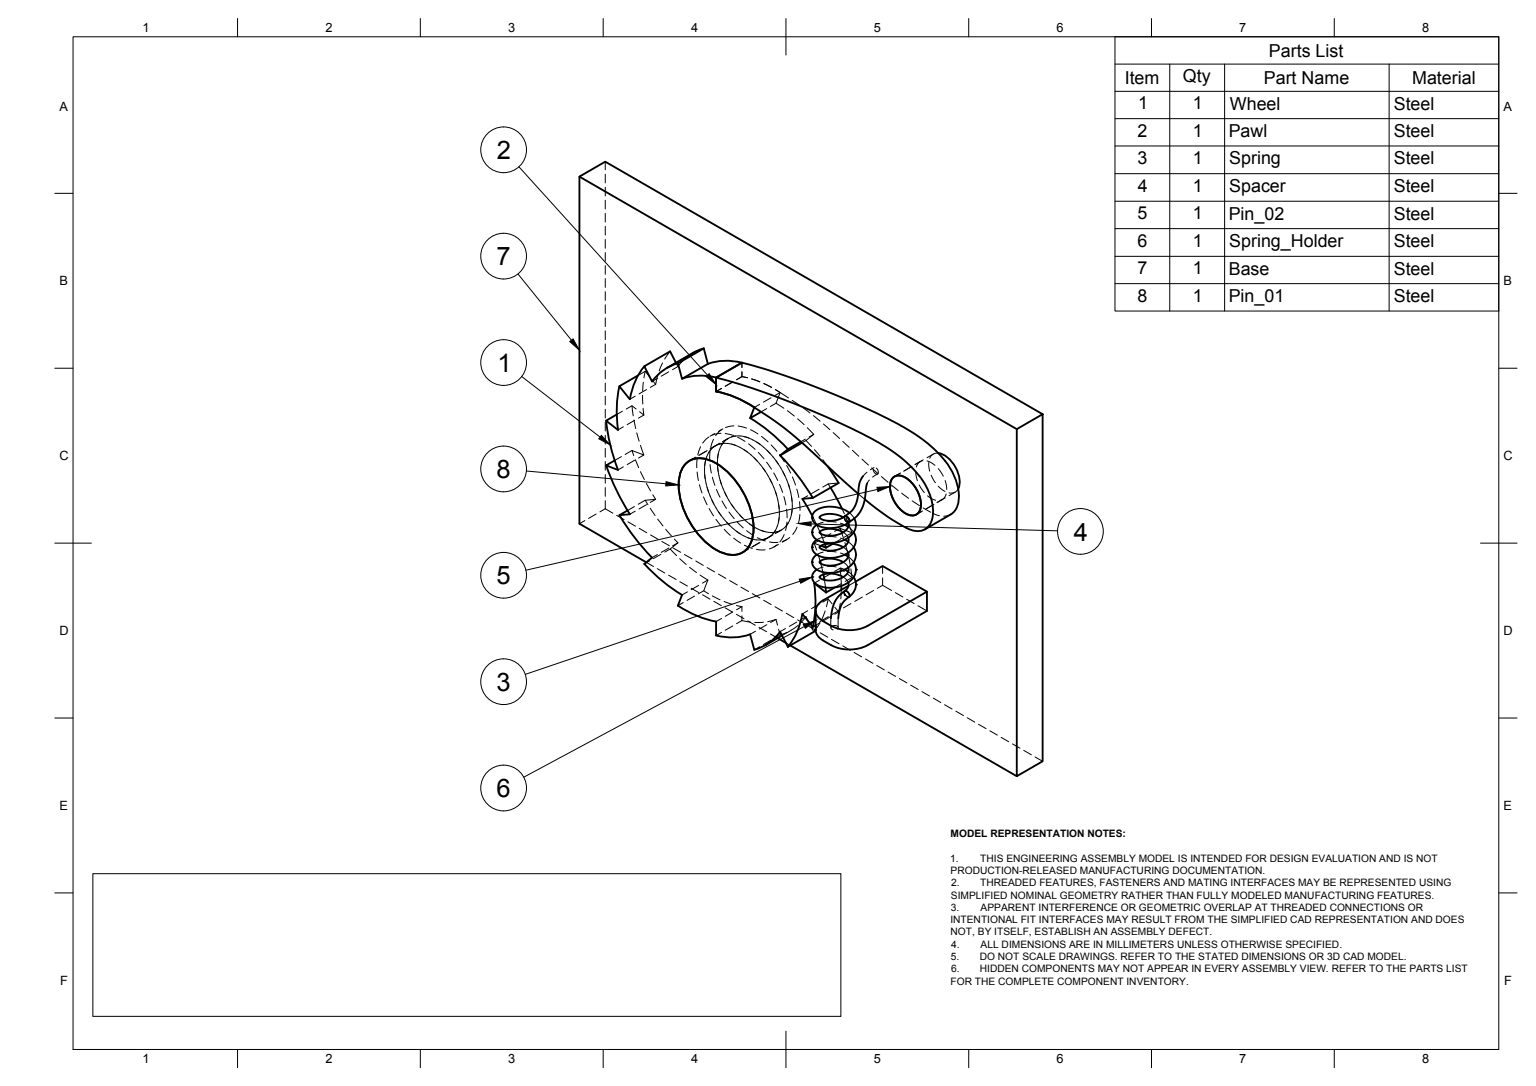
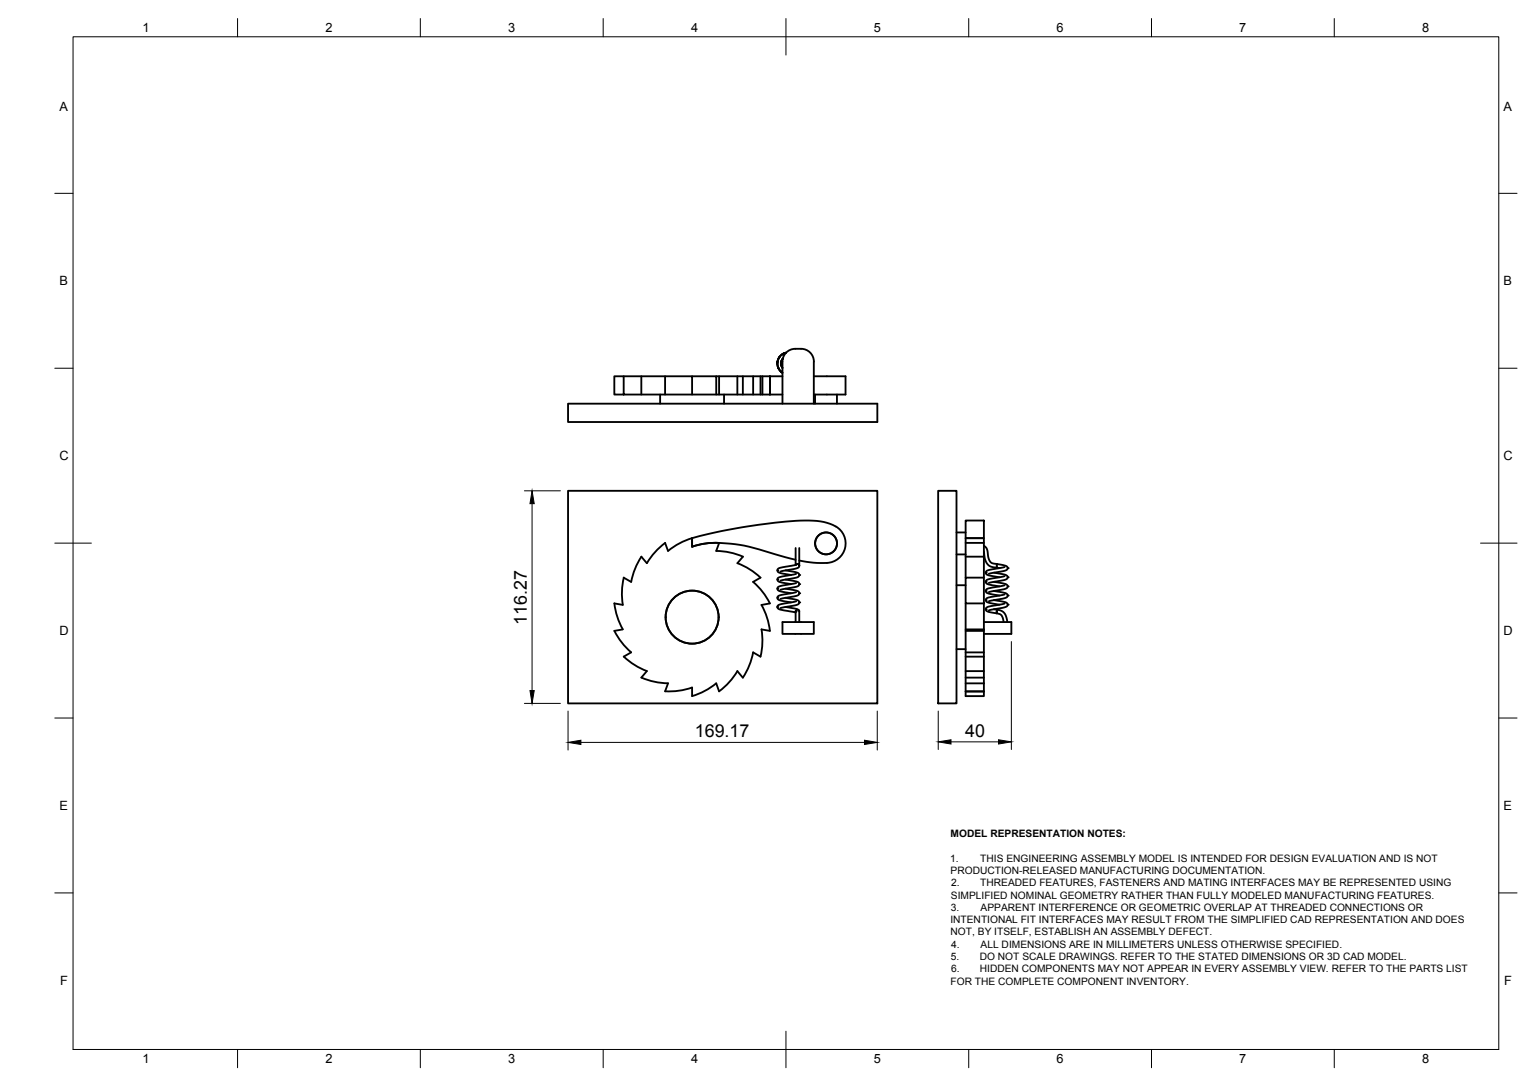
ISO-10303-21;
HEADER;
/* Generated by software containing ST-Developer
 * from STEP Tools, Inc. (www.steptools.com) 
 */

FILE_DESCRIPTION(
/* description */ (''),
/* implementation_level */ '2;1');

FILE_NAME(
/* name */ 'BR-055',
/* time_stamp */ '2026-09-20T22:38:01+06:00',
/* author */ (''),
/* organization */ (''),
/* preprocessor_version */ 'ST-DEVELOPER v20.2',
/* originating_system */ 'Autodesk Translation Framework v15.15.0.0',
/* authorisation */ '');

FILE_SCHEMA (('AUTOMOTIVE_DESIGN { 1 0 10303 214 3 1 1 }'));
ENDSEC;

DATA;
#10=MECHANICAL_DESIGN_GEOMETRIC_PRESENTATION_REPRESENTATION('',(#84,#85,
#86,#87,#88,#89,#90,#91),#4079);
#11=ITEM_DEFINED_TRANSFORMATION($,$,#1541,#1690);
#12=ITEM_DEFINED_TRANSFORMATION($,$,#1619,#1691);
#13=ITEM_DEFINED_TRANSFORMATION($,$,#1632,#1692);
#14=ITEM_DEFINED_TRANSFORMATION($,$,#1649,#1693);
#15=ITEM_DEFINED_TRANSFORMATION($,$,#1658,#1694);
#16=ITEM_DEFINED_TRANSFORMATION($,$,#1664,#1695);
#17=ITEM_DEFINED_TRANSFORMATION($,$,#1677,#1696);
#18=ITEM_DEFINED_TRANSFORMATION($,$,#1684,#1697);
#19=(
REPRESENTATION_RELATIONSHIP($,$,#4111,#4110)
REPRESENTATION_RELATIONSHIP_WITH_TRANSFORMATION(#11)
SHAPE_REPRESENTATION_RELATIONSHIP()
);
#20=(
REPRESENTATION_RELATIONSHIP($,$,#4112,#4110)
REPRESENTATION_RELATIONSHIP_WITH_TRANSFORMATION(#12)
SHAPE_REPRESENTATION_RELATIONSHIP()
);
#21=(
REPRESENTATION_RELATIONSHIP($,$,#4113,#4110)
REPRESENTATION_RELATIONSHIP_WITH_TRANSFORMATION(#13)
SHAPE_REPRESENTATION_RELATIONSHIP()
);
#22=(
REPRESENTATION_RELATIONSHIP($,$,#4114,#4110)
REPRESENTATION_RELATIONSHIP_WITH_TRANSFORMATION(#14)
SHAPE_REPRESENTATION_RELATIONSHIP()
);
#23=(
REPRESENTATION_RELATIONSHIP($,$,#4115,#4110)
REPRESENTATION_RELATIONSHIP_WITH_TRANSFORMATION(#15)
SHAPE_REPRESENTATION_RELATIONSHIP()
);
#24=(
REPRESENTATION_RELATIONSHIP($,$,#4116,#4110)
REPRESENTATION_RELATIONSHIP_WITH_TRANSFORMATION(#16)
SHAPE_REPRESENTATION_RELATIONSHIP()
);
#25=(
REPRESENTATION_RELATIONSHIP($,$,#4117,#4110)
REPRESENTATION_RELATIONSHIP_WITH_TRANSFORMATION(#17)
SHAPE_REPRESENTATION_RELATIONSHIP()
);
#26=(
REPRESENTATION_RELATIONSHIP($,$,#4118,#4110)
REPRESENTATION_RELATIONSHIP_WITH_TRANSFORMATION(#18)
SHAPE_REPRESENTATION_RELATIONSHIP()
);
#27=CONTEXT_DEPENDENT_SHAPE_REPRESENTATION(#19,#4102);
#28=CONTEXT_DEPENDENT_SHAPE_REPRESENTATION(#20,#4103);
#29=CONTEXT_DEPENDENT_SHAPE_REPRESENTATION(#21,#4104);
#30=CONTEXT_DEPENDENT_SHAPE_REPRESENTATION(#22,#4105);
#31=CONTEXT_DEPENDENT_SHAPE_REPRESENTATION(#23,#4106);
#32=CONTEXT_DEPENDENT_SHAPE_REPRESENTATION(#24,#4107);
#33=CONTEXT_DEPENDENT_SHAPE_REPRESENTATION(#25,#4108);
#34=CONTEXT_DEPENDENT_SHAPE_REPRESENTATION(#26,#4109);
#35=NEXT_ASSEMBLY_USAGE_OCCURRENCE('Wheel:1','Wheel:1','Wheel:1',#4120,
#4121,'Wheel:1');
#36=NEXT_ASSEMBLY_USAGE_OCCURRENCE('Pawl:1','Pawl:1','Pawl:1',#4120,#4122,
'Pawl:1');
#37=NEXT_ASSEMBLY_USAGE_OCCURRENCE('Spring:1','Spring:1','Spring:1',#4120,
#4123,'Spring:1');
#38=NEXT_ASSEMBLY_USAGE_OCCURRENCE('Spacer:1','Spacer:1','Spacer:1',#4120,
#4124,'Spacer:1');
#39=NEXT_ASSEMBLY_USAGE_OCCURRENCE('Pin_02:1','Pin_02:1','Pin_02:1',#4120,
#4125,'Pin_02:1');
#40=NEXT_ASSEMBLY_USAGE_OCCURRENCE('Spring_Holder:1','Spring_Holder:1',
'Spring_Holder:1',#4120,#4126,'Spring_Holder:1');
#41=NEXT_ASSEMBLY_USAGE_OCCURRENCE('Base:1','Base:1','Base:1',#4120,#4127,
'Base:1');
#42=NEXT_ASSEMBLY_USAGE_OCCURRENCE('Pin_01:1','Pin_01:1','Pin_01:1',#4120,
#4128,'Pin_01:1');
#43=B_SPLINE_CURVE_WITH_KNOTS('',3,(#2659,#2660,#2661,#2662,#2663,#2664,
#2665,#2666,#2667,#2668,#2669,#2670,#2671,#2672,#2673,#2674,#2675,#2676,
#2677,#2678,#2679,#2680,#2681,#2682,#2683,#2684,#2685,#2686),
 .UNSPECIFIED.,.F.,.F.,(4,3,3,3,3,3,3,3,3,4),(-0.465553767595507,-0.45230342916427,
-0.438736142747031,-0.431079433868877,-0.417558478811202,-0.404199900672923,
-0.391686604552913,-0.378322214394046,-0.374830772248012,-0.369773118077988),
 .UNSPECIFIED.);
#44=B_SPLINE_CURVE_WITH_KNOTS('',3,(#2688,#2689,#2690,#2691,#2692,#2693,
#2694,#2695,#2696,#2697),.UNSPECIFIED.,.F.,.F.,(4,2,2,2,4),(-0.09742200167385,
-0.0775242929113368,-0.0386624365460309,0.,0.00241811618144354),
 .UNSPECIFIED.);
#45=B_SPLINE_CURVE_WITH_KNOTS('',3,(#2702,#2703,#2704,#2705,#2706,#2707,
#2708,#2709,#2710,#2711),.UNSPECIFIED.,.F.,.F.,(4,3,3,4),(-0.657219142658169,
-0.648664678619421,-0.598426048115365,-0.569492481999336),.UNSPECIFIED.);
#46=B_SPLINE_CURVE_WITH_KNOTS('',3,(#2712,#2713,#2714,#2715,#2716,#2717,
#2718,#2719,#2720,#2721),.UNSPECIFIED.,.F.,.F.,(4,3,3,4),(-0.489269526390867,
-0.47602824474659,-0.470821216724862,-0.465553767595507),.UNSPECIFIED.);
#47=B_SPLINE_CURVE_WITH_KNOTS('',3,(#2723,#2724,#2725,#2726,#2727,#2728,
#2729,#2730,#2731),.UNSPECIFIED.,.F.,.F.,(4,1,1,1,1,1,4),(0.0132171477861262,
0.142857142857143,0.285714285714286,0.428571428571429,0.571428571428571,
0.857142857142857,1.),.UNSPECIFIED.);
#48=B_SPLINE_CURVE_WITH_KNOTS('',3,(#3403,#3404,#3405,#3406,#3407,#3408,
#3409,#3410,#3411,#3412,#3413,#3414,#3415,#3416,#3417,#3418,#3419,#3420,
#3421,#3422,#3423,#3424,#3425),.UNSPECIFIED.,.F.,.F.,(4,2,3,2,2,2,2,2,2,
2,4),(0.587267836178956,0.604560146171109,0.626248329271999,0.664698946888708,
0.70347541138122,0.74264809527987,0.78210152700143,0.821492769940296,0.860375715352057,
0.898588405045022,0.900352617840992),.UNSPECIFIED.);
#49=B_SPLINE_CURVE_WITH_KNOTS('',3,(#3427,#3428,#3429,#3430,#3431,#3432,
#3433,#3434,#3435,#3436,#3437,#3438,#3439,#3440,#3441,#3442,#3443,#3444,
#3445,#3446,#3447,#3448,#3449,#3450,#3451,#3452,#3453,#3454,#3455,#3456,
#3457,#3458,#3459,#3460,#3461,#3462,#3463,#3464,#3465,#3466,#3467,#3468,
#3469,#3470,#3471,#3472,#3473,#3474,#3475,#3476,#3477,#3478,#3479,#3480,
#3481,#3482,#3483,#3484,#3485,#3486,#3487,#3488,#3489,#3490,#3491,#3492,
#3493),.UNSPECIFIED.,.F.,.F.,(4,1,1,1,1,1,1,1,1,1,1,1,1,1,1,1,1,1,1,1,1,
1,1,1,1,1,1,1,1,1,1,1,1,1,1,1,1,1,1,1,1,1,1,1,1,1,1,1,1,1,1,1,1,1,1,1,1,
1,1,1,1,1,1,1,4),(0.,0.464577110944849,0.95586837165839,1.44715963237193,
1.93845089308547,2.42974215379901,2.92103341451255,3.41232467522609,3.90361593593964,
4.39490719665318,4.88619845736672,5.37748971808026,5.8687809787938,6.36007223950734,
6.85136350022088,7.34265476093442,7.83394602164796,8.3252372823615,8.81652854307505,
9.30781980378859,9.79911106450213,10.2904023252157,10.7816935859292,11.2729848466427,
11.7642761073563,12.2555673680698,12.7468586287834,13.2381498894969,13.7294411502105,
14.220732410924,14.7120236716375,15.2033149323511,15.6946061930646,16.1858974537782,
16.6771887144917,17.1684799752052,17.6597712359188,18.1510624966323,18.6423537573459,
19.1336450180594,19.6249362787729,20.1162275394865,20.6075188002,21.0988100609136,
21.5901013216271,22.0813925823407,22.5726838430542,23.0639751037677,23.5552663644813,
24.0465576251948,24.5378488859084,25.0291401466219,25.5204314073354,26.011722668049,
26.5030139287625,26.9943051894761,27.4855964501896,27.9768877109031,28.4681789716167,
28.9594702323302,29.4507614930438,29.9420527537573,30.4333440144708,30.9246352751844,
31.4159265358979),.UNSPECIFIED.);
#50=B_SPLINE_CURVE_WITH_KNOTS('',3,(#3495,#3496,#3497,#3498,#3499,#3500,
#3501,#3502,#3503,#3504,#3505,#3506,#3507,#3508,#3509,#3510,#3511,#3512,
#3513,#3514),.UNSPECIFIED.,.F.,.F.,(4,2,2,2,2,2,2,2,2,4),(-0.313052705156199,
-0.292609441796844,-0.272153993775093,-0.233472325120928,-0.194370984993977,
-0.154905297587714,-0.115391052867927,-0.0763129985395409,-0.0379453287021336,
0.),.UNSPECIFIED.);
#51=B_SPLINE_CURVE_WITH_KNOTS('',3,(#3516,#3517,#3518,#3519,#3520,#3521,
#3522,#3523,#3524,#3525,#3526,#3527,#3528,#3529,#3530,#3531),
 .UNSPECIFIED.,.F.,.F.,(4,3,3,3,3,4),(-0.0024248849541149,0.,0.0138283319525736,
0.0273768962823761,0.0362935842092716,0.0434201122759664),.UNSPECIFIED.);
#52=B_SPLINE_CURVE_WITH_KNOTS('',3,(#3533,#3534,#3535,#3536,#3537,#3538),
 .UNSPECIFIED.,.F.,.F.,(4,2,4),(-0.0515505060017679,-0.0391387739403107,
0.),.UNSPECIFIED.);
#53=B_SPLINE_CURVE_WITH_KNOTS('',3,(#3542,#3543,#3544,#3545,#3546,#3547,
#3548,#3549,#3550,#3551,#3552,#3553,#3554,#3555,#3556,#3557,#3558,#3559,
#3560,#3561),.UNSPECIFIED.,.F.,.F.,(4,2,2,2,2,2,2,2,2,4),(-0.313052705156207,
-0.29260944179685,-0.272153993775096,-0.233472325120924,-0.194370984993967,
-0.154905297587702,-0.11539105286792,-0.0763129985395404,-0.0379453287021338,
0.),.UNSPECIFIED.);
#54=B_SPLINE_CURVE_WITH_KNOTS('',3,(#3563,#3564,#3565,#3566,#3567,#3568,
#3569,#3570,#3571,#3572,#3573,#3574,#3575,#3576,#3577,#3578,#3579,#3580,
#3581,#3582,#3583,#3584,#3585,#3586,#3587,#3588,#3589,#3590,#3591,#3592,
#3593,#3594,#3595,#3596),.UNSPECIFIED.,.F.,.F.,(4,3,3,3,3,3,3,3,3,3,3,4),
(0.377352254196932,0.390588465654341,0.403867575958707,0.41718187397498,
0.429352359462404,0.437218808334642,0.450427222970435,0.463782588613302,
0.468146972739535,0.481501401691605,0.494833441685106,0.497267224677679),
 .UNSPECIFIED.);
#55=B_SPLINE_CURVE_WITH_KNOTS('',3,(#3600,#3601,#3602,#3603,#3604,#3605,
#3606,#3607,#3608,#3609,#3610,#3611,#3612,#3613,#3614,#3615,#3616,#3617,
#3618,#3619,#3620,#3621,#3622,#3623,#3624,#3625,#3626,#3627),
 .UNSPECIFIED.,.F.,.F.,(4,3,3,3,3,3,3,3,3,4),(0.458621120799817,0.464048968999107,
0.469643578756217,0.482746851650584,0.496256676637028,0.508878670584022,
0.522421915099756,0.535791652499991,0.548459753273671,0.554671659389392),
 .UNSPECIFIED.);
#56=B_SPLINE_CURVE_WITH_KNOTS('',3,(#3888,#3889,#3890,#3891,#3892,#3893,
#3894,#3895,#3896,#3897),.UNSPECIFIED.,.F.,.F.,(4,3,3,4),(-0.319964114535563,
-0.319531325306217,-0.229500308639694,-0.144878157103041),.UNSPECIFIED.);
#57=B_SPLINE_CURVE_WITH_KNOTS('',3,(#3900,#3901,#3902,#3903,#3904,#3905,
#3906,#3907,#3908,#3909,#3910,#3911,#3912,#3913,#3914,#3915,#3916,#3917,
#3918,#3919,#3920,#3921,#3922,#3923),.UNSPECIFIED.,.F.,.F.,(4,1,1,1,1,1,
1,1,1,1,1,1,1,1,1,1,1,1,1,1,1,4),(0.,0.025,0.05,0.1,0.15,0.175,0.2,0.3,
0.4,0.425,0.45,0.5,0.55,0.575,0.6,0.7,0.75,0.8,0.825,0.85,0.9,1.),
 .UNSPECIFIED.);
#58=B_SPLINE_SURFACE_WITH_KNOTS('',3,3,((#2567,#2568,#2569,#2570,#2571,
#2572,#2573,#2574,#2575),(#2576,#2577,#2578,#2579,#2580,#2581,#2582,#2583,
#2584),(#2585,#2586,#2587,#2588,#2589,#2590,#2591,#2592,#2593),(#2594,#2595,
#2596,#2597,#2598,#2599,#2600,#2601,#2602),(#2603,#2604,#2605,#2606,#2607,
#2608,#2609,#2610,#2611),(#2612,#2613,#2614,#2615,#2616,#2617,#2618,#2619,
#2620),(#2621,#2622,#2623,#2624,#2625,#2626,#2627,#2628,#2629),(#2630,#2631,
#2632,#2633,#2634,#2635,#2636,#2637,#2638),(#2639,#2640,#2641,#2642,#2643,
#2644,#2645,#2646,#2647),(#2648,#2649,#2650,#2651,#2652,#2653,#2654,#2655,
#2656)),.UNSPECIFIED.,.T.,.F.,.F.,(4,1,1,1,1,1,1,4),(4,1,1,1,1,1,4),(-3.14159265359034,
-2.2439947525646,-1.34639685153886,-0.448798950513122,0.448798950512615,
1.34639685153835,2.24399475256409,3.14159265358983),(0.,0.142857142857143,
0.285714285714286,0.428571428571429,0.571428571428571,0.857142857142857,
1.),.UNSPECIFIED.);
#59=B_SPLINE_SURFACE_WITH_KNOTS('',3,3,((#2733,#2734,#2735,#2736,#2737,
#2738,#2739,#2740,#2741,#2742,#2743,#2744,#2745,#2746,#2747,#2748,#2749,
#2750,#2751,#2752,#2753,#2754,#2755,#2756,#2757,#2758,#2759,#2760,#2761,
#2762,#2763,#2764,#2765,#2766,#2767,#2768,#2769,#2770,#2771,#2772,#2773,
#2774,#2775,#2776,#2777,#2778,#2779,#2780,#2781,#2782,#2783,#2784,#2785,
#2786,#2787,#2788,#2789,#2790,#2791,#2792,#2793,#2794,#2795,#2796,#2797,
#2798,#2799),(#2800,#2801,#2802,#2803,#2804,#2805,#2806,#2807,#2808,#2809,
#2810,#2811,#2812,#2813,#2814,#2815,#2816,#2817,#2818,#2819,#2820,#2821,
#2822,#2823,#2824,#2825,#2826,#2827,#2828,#2829,#2830,#2831,#2832,#2833,
#2834,#2835,#2836,#2837,#2838,#2839,#2840,#2841,#2842,#2843,#2844,#2845,
#2846,#2847,#2848,#2849,#2850,#2851,#2852,#2853,#2854,#2855,#2856,#2857,
#2858,#2859,#2860,#2861,#2862,#2863,#2864,#2865,#2866),(#2867,#2868,#2869,
#2870,#2871,#2872,#2873,#2874,#2875,#2876,#2877,#2878,#2879,#2880,#2881,
#2882,#2883,#2884,#2885,#2886,#2887,#2888,#2889,#2890,#2891,#2892,#2893,
#2894,#2895,#2896,#2897,#2898,#2899,#2900,#2901,#2902,#2903,#2904,#2905,
#2906,#2907,#2908,#2909,#2910,#2911,#2912,#2913,#2914,#2915,#2916,#2917,
#2918,#2919,#2920,#2921,#2922,#2923,#2924,#2925,#2926,#2927,#2928,#2929,
#2930,#2931,#2932,#2933),(#2934,#2935,#2936,#2937,#2938,#2939,#2940,#2941,
#2942,#2943,#2944,#2945,#2946,#2947,#2948,#2949,#2950,#2951,#2952,#2953,
#2954,#2955,#2956,#2957,#2958,#2959,#2960,#2961,#2962,#2963,#2964,#2965,
#2966,#2967,#2968,#2969,#2970,#2971,#2972,#2973,#2974,#2975,#2976,#2977,
#2978,#2979,#2980,#2981,#2982,#2983,#2984,#2985,#2986,#2987,#2988,#2989,
#2990,#2991,#2992,#2993,#2994,#2995,#2996,#2997,#2998,#2999,#3000),(#3001,
#3002,#3003,#3004,#3005,#3006,#3007,#3008,#3009,#3010,#3011,#3012,#3013,
#3014,#3015,#3016,#3017,#3018,#3019,#3020,#3021,#3022,#3023,#3024,#3025,
#3026,#3027,#3028,#3029,#3030,#3031,#3032,#3033,#3034,#3035,#3036,#3037,
#3038,#3039,#3040,#3041,#3042,#3043,#3044,#3045,#3046,#3047,#3048,#3049,
#3050,#3051,#3052,#3053,#3054,#3055,#3056,#3057,#3058,#3059,#3060,#3061,
#3062,#3063,#3064,#3065,#3066,#3067),(#3068,#3069,#3070,#3071,#3072,#3073,
#3074,#3075,#3076,#3077,#3078,#3079,#3080,#3081,#3082,#3083,#3084,#3085,
#3086,#3087,#3088,#3089,#3090,#3091,#3092,#3093,#3094,#3095,#3096,#3097,
#3098,#3099,#3100,#3101,#3102,#3103,#3104,#3105,#3106,#3107,#3108,#3109,
#3110,#3111,#3112,#3113,#3114,#3115,#3116,#3117,#3118,#3119,#3120,#3121,
#3122,#3123,#3124,#3125,#3126,#3127,#3128,#3129,#3130,#3131,#3132,#3133,
#3134),(#3135,#3136,#3137,#3138,#3139,#3140,#3141,#3142,#3143,#3144,#3145,
#3146,#3147,#3148,#3149,#3150,#3151,#3152,#3153,#3154,#3155,#3156,#3157,
#3158,#3159,#3160,#3161,#3162,#3163,#3164,#3165,#3166,#3167,#3168,#3169,
#3170,#3171,#3172,#3173,#3174,#3175,#3176,#3177,#3178,#3179,#3180,#3181,
#3182,#3183,#3184,#3185,#3186,#3187,#3188,#3189,#3190,#3191,#3192,#3193,
#3194,#3195,#3196,#3197,#3198,#3199,#3200,#3201),(#3202,#3203,#3204,#3205,
#3206,#3207,#3208,#3209,#3210,#3211,#3212,#3213,#3214,#3215,#3216,#3217,
#3218,#3219,#3220,#3221,#3222,#3223,#3224,#3225,#3226,#3227,#3228,#3229,
#3230,#3231,#3232,#3233,#3234,#3235,#3236,#3237,#3238,#3239,#3240,#3241,
#3242,#3243,#3244,#3245,#3246,#3247,#3248,#3249,#3250,#3251,#3252,#3253,
#3254,#3255,#3256,#3257,#3258,#3259,#3260,#3261,#3262,#3263,#3264,#3265,
#3266,#3267,#3268),(#3269,#3270,#3271,#3272,#3273,#3274,#3275,#3276,#3277,
#3278,#3279,#3280,#3281,#3282,#3283,#3284,#3285,#3286,#3287,#3288,#3289,
#3290,#3291,#3292,#3293,#3294,#3295,#3296,#3297,#3298,#3299,#3300,#3301,
#3302,#3303,#3304,#3305,#3306,#3307,#3308,#3309,#3310,#3311,#3312,#3313,
#3314,#3315,#3316,#3317,#3318,#3319,#3320,#3321,#3322,#3323,#3324,#3325,
#3326,#3327,#3328,#3329,#3330,#3331,#3332,#3333,#3334,#3335),(#3336,#3337,
#3338,#3339,#3340,#3341,#3342,#3343,#3344,#3345,#3346,#3347,#3348,#3349,
#3350,#3351,#3352,#3353,#3354,#3355,#3356,#3357,#3358,#3359,#3360,#3361,
#3362,#3363,#3364,#3365,#3366,#3367,#3368,#3369,#3370,#3371,#3372,#3373,
#3374,#3375,#3376,#3377,#3378,#3379,#3380,#3381,#3382,#3383,#3384,#3385,
#3386,#3387,#3388,#3389,#3390,#3391,#3392,#3393,#3394,#3395,#3396,#3397,
#3398,#3399,#3400,#3401,#3402)),.UNSPECIFIED.,.T.,.F.,.F.,(4,1,1,1,1,1,
1,4),(4,1,1,1,1,1,1,1,1,1,1,1,1,1,1,1,1,1,1,1,1,1,1,1,1,1,1,1,1,1,1,1,1,
1,1,1,1,1,1,1,1,1,1,1,1,1,1,1,1,1,1,1,1,1,1,1,1,1,1,1,1,1,1,1,4),(-3.14159265358979,
-2.24399475256414,-1.34639685153848,-0.448798950512828,0.448798950512828,
1.34639685153848,2.24399475256414,3.14159265358979),(-0.0267141497686917,
0.464577110944849,0.95586837165839,1.44715963237193,1.93845089308547,2.42974215379901,
2.92103341451255,3.41232467522609,3.90361593593964,4.39490719665318,4.88619845736672,
5.37748971808026,5.8687809787938,6.36007223950734,6.85136350022088,7.34265476093442,
7.83394602164796,8.3252372823615,8.81652854307505,9.30781980378859,9.79911106450213,
10.2904023252157,10.7816935859292,11.2729848466427,11.7642761073563,12.2555673680698,
12.7468586287834,13.2381498894969,13.7294411502105,14.220732410924,14.7120236716375,
15.2033149323511,15.6946061930646,16.1858974537782,16.6771887144917,17.1684799752052,
17.6597712359188,18.1510624966323,18.6423537573459,19.1336450180594,19.6249362787729,
20.1162275394865,20.6075188002,21.0988100609136,21.5901013216271,22.0813925823407,
22.5726838430542,23.0639751037677,23.5552663644813,24.0465576251948,24.5378488859084,
25.0291401466219,25.5204314073354,26.011722668049,26.5030139287625,26.9943051894761,
27.4855964501896,27.9768877109031,28.4681789716167,28.9594702323302,29.4507614930438,
29.9420527537573,30.4333440144708,30.9246352751844,31.4159265358979),
 .UNSPECIFIED.);
#60=B_SPLINE_SURFACE_WITH_KNOTS('',3,3,((#3628,#3629,#3630,#3631,#3632,
#3633,#3634,#3635,#3636,#3637,#3638,#3639,#3640,#3641,#3642,#3643,#3644,
#3645,#3646,#3647,#3648,#3649,#3650,#3651,#3652,#3653),(#3654,#3655,#3656,
#3657,#3658,#3659,#3660,#3661,#3662,#3663,#3664,#3665,#3666,#3667,#3668,
#3669,#3670,#3671,#3672,#3673,#3674,#3675,#3676,#3677,#3678,#3679),(#3680,
#3681,#3682,#3683,#3684,#3685,#3686,#3687,#3688,#3689,#3690,#3691,#3692,
#3693,#3694,#3695,#3696,#3697,#3698,#3699,#3700,#3701,#3702,#3703,#3704,
#3705),(#3706,#3707,#3708,#3709,#3710,#3711,#3712,#3713,#3714,#3715,#3716,
#3717,#3718,#3719,#3720,#3721,#3722,#3723,#3724,#3725,#3726,#3727,#3728,
#3729,#3730,#3731),(#3732,#3733,#3734,#3735,#3736,#3737,#3738,#3739,#3740,
#3741,#3742,#3743,#3744,#3745,#3746,#3747,#3748,#3749,#3750,#3751,#3752,
#3753,#3754,#3755,#3756,#3757),(#3758,#3759,#3760,#3761,#3762,#3763,#3764,
#3765,#3766,#3767,#3768,#3769,#3770,#3771,#3772,#3773,#3774,#3775,#3776,
#3777,#3778,#3779,#3780,#3781,#3782,#3783),(#3784,#3785,#3786,#3787,#3788,
#3789,#3790,#3791,#3792,#3793,#3794,#3795,#3796,#3797,#3798,#3799,#3800,
#3801,#3802,#3803,#3804,#3805,#3806,#3807,#3808,#3809),(#3810,#3811,#3812,
#3813,#3814,#3815,#3816,#3817,#3818,#3819,#3820,#3821,#3822,#3823,#3824,
#3825,#3826,#3827,#3828,#3829,#3830,#3831,#3832,#3833,#3834,#3835),(#3836,
#3837,#3838,#3839,#3840,#3841,#3842,#3843,#3844,#3845,#3846,#3847,#3848,
#3849,#3850,#3851,#3852,#3853,#3854,#3855,#3856,#3857,#3858,#3859,#3860,
#3861),(#3862,#3863,#3864,#3865,#3866,#3867,#3868,#3869,#3870,#3871,#3872,
#3873,#3874,#3875,#3876,#3877,#3878,#3879,#3880,#3881,#3882,#3883,#3884,
#3885,#3886,#3887)),.UNSPECIFIED.,.T.,.F.,.F.,(4,1,1,1,1,1,1,4),(4,2,1,
1,1,1,1,1,1,1,1,1,1,1,1,1,1,1,1,1,1,1,4),(-3.14159265358979,-2.24399475256414,
-1.34639685153848,-0.448798950512828,0.448798950512828,1.34639685153848,
2.24399475256414,3.14159265358979),(-0.00680747846147418,0.,0.025,0.05,
0.1,0.15,0.175,0.2,0.3,0.4,0.425,0.45,0.5,0.55,0.575,0.6,0.7,0.75,0.8,0.825,
0.85,0.9,1.),.UNSPECIFIED.);
#61=B_SPLINE_SURFACE_WITH_KNOTS('',3,3,((#3925,#3926,#3927,#3928),(#3929,
#3930,#3931,#3932),(#3933,#3934,#3935,#3936),(#3937,#3938,#3939,#3940),
(#3941,#3942,#3943,#3944)),.UNSPECIFIED.,.F.,.F.,.F.,(4,1,4),(4,4),(-0.950877784735382,
-0.352362581588169,0.246152621559044),(-0.0375396701634702,0.),
 .UNSPECIFIED.);
#62=(
BOUNDED_CURVE()
B_SPLINE_CURVE(5,(#2402,#2403,#2404,#2405,#2406,#2407,#2408,#2409,#2410,
#2411,#2412,#2413,#2414,#2415,#2416,#2417,#2418,#2419,#2420,#2421),
 .UNSPECIFIED.,.F.,.F.)
B_SPLINE_CURVE_WITH_KNOTS((6,1,1,1,1,1,1,1,1,1,1,1,1,1,1,6),(0.,0.0666666666666667,
0.133333333333333,0.2,0.266666666666667,0.333333333333333,0.4,0.466666666666667,
0.533333333333333,0.6,0.666666666666667,0.733333333333333,0.8,0.866666666666667,
0.933333333333333,1.),.UNSPECIFIED.)
CURVE()
GEOMETRIC_REPRESENTATION_ITEM()
RATIONAL_B_SPLINE_CURVE((1.,1.,1.,1.,1.,1.,1.,1.,1.,1.,1.,1.,1.,1.,1.,1.,
1.,1.,1.,1.))
REPRESENTATION_ITEM('')
);
#63=(
BOUNDED_CURVE()
B_SPLINE_CURVE(5,(#2425,#2426,#2427,#2428,#2429,#2430,#2431,#2432,#2433,
#2434,#2435,#2436,#2437,#2438,#2439,#2440,#2441,#2442,#2443,#2444),
 .UNSPECIFIED.,.F.,.F.)
B_SPLINE_CURVE_WITH_KNOTS((6,1,1,1,1,1,1,1,1,1,1,1,1,1,1,6),(-1.,-0.933333333333333,
-0.866666666666667,-0.8,-0.733333333333333,-0.666666666666667,-0.6,-0.533333333333333,
-0.466666666666667,-0.4,-0.333333333333333,-0.266666666666667,-0.2,-0.133333333333333,
-0.0666666666666667,0.),.UNSPECIFIED.)
CURVE()
GEOMETRIC_REPRESENTATION_ITEM()
RATIONAL_B_SPLINE_CURVE((1.,1.,1.,1.,1.,1.,1.,1.,1.,1.,1.,1.,1.,1.,1.,1.,
1.,1.,1.,1.))
REPRESENTATION_ITEM('')
);
#64=(
BOUNDED_CURVE()
B_SPLINE_CURVE(5,(#2503,#2504,#2505,#2506,#2507,#2508,#2509,#2510,#2511,
#2512,#2513,#2514,#2515,#2516,#2517,#2518,#2519,#2520,#2521,#2522,#2523,
#2524,#2525,#2526,#2527),.UNSPECIFIED.,.F.,.F.)
B_SPLINE_CURVE_WITH_KNOTS((6,1,1,1,1,1,1,1,1,1,1,1,1,1,1,1,1,1,1,1,6),(0.,
0.05,0.1,0.15,0.2,0.25,0.3,0.35,0.4,0.45,0.5,0.55,0.6,0.65,0.7,0.75,0.8,
0.85,0.9,0.95,1.),.UNSPECIFIED.)
CURVE()
GEOMETRIC_REPRESENTATION_ITEM()
RATIONAL_B_SPLINE_CURVE((1.,1.,1.,1.,1.,1.,1.,1.,1.,1.,1.,1.,1.,1.,1.,1.,
1.,1.,1.,1.,1.,1.,1.,1.,1.))
REPRESENTATION_ITEM('')
);
#65=(
BOUNDED_CURVE()
B_SPLINE_CURVE(5,(#2529,#2530,#2531,#2532,#2533,#2534,#2535,#2536,#2537,
#2538,#2539,#2540,#2541,#2542,#2543,#2544,#2545,#2546,#2547,#2548,#2549,
#2550,#2551,#2552,#2553),.UNSPECIFIED.,.F.,.F.)
B_SPLINE_CURVE_WITH_KNOTS((6,1,1,1,1,1,1,1,1,1,1,1,1,1,1,1,1,1,1,1,6),(0.,
0.05,0.1,0.15,0.2,0.25,0.3,0.35,0.4,0.45,0.5,0.55,0.6,0.65,0.7,0.75,0.8,
0.85,0.9,0.95,1.),.UNSPECIFIED.)
CURVE()
GEOMETRIC_REPRESENTATION_ITEM()
RATIONAL_B_SPLINE_CURVE((1.,1.,1.,1.,1.,1.,1.,1.,1.,1.,1.,1.,1.,1.,1.,1.,
1.,1.,1.,1.,1.,1.,1.,1.,1.))
REPRESENTATION_ITEM('')
);
#66=(
BOUNDED_SURFACE()
B_SPLINE_SURFACE(5,1,((#2360,#2361),(#2362,#2363),(#2364,#2365),(#2366,
#2367),(#2368,#2369),(#2370,#2371),(#2372,#2373),(#2374,#2375),(#2376,#2377),
(#2378,#2379),(#2380,#2381),(#2382,#2383),(#2384,#2385),(#2386,#2387),(#2388,
#2389),(#2390,#2391),(#2392,#2393),(#2394,#2395),(#2396,#2397),(#2398,#2399)),
 .UNSPECIFIED.,.F.,.F.,.F.)
B_SPLINE_SURFACE_WITH_KNOTS((6,1,1,1,1,1,1,1,1,1,1,1,1,1,1,6),(2,2),(-1.,
-0.933333333333333,-0.866666666666667,-0.8,-0.733333333333333,-0.666666666666667,
-0.6,-0.533333333333333,-0.466666666666667,-0.4,-0.333333333333333,-0.266666666666667,
-0.2,-0.133333333333333,-0.0666666666666667,0.),(0.,1.),.UNSPECIFIED.)
GEOMETRIC_REPRESENTATION_ITEM()
RATIONAL_B_SPLINE_SURFACE(((1.,1.),(1.,1.),(1.,1.),(1.,1.),(1.,1.),(1.,
1.),(1.,1.),(1.,1.),(1.,1.),(1.,1.),(1.,1.),(1.,1.),(1.,1.),(1.,1.),(1.,
1.),(1.,1.),(1.,1.),(1.,1.),(1.,1.),(1.,1.)))
REPRESENTATION_ITEM('')
SURFACE()
);
#67=(
BOUNDED_SURFACE()
B_SPLINE_SURFACE(5,1,((#2452,#2453),(#2454,#2455),(#2456,#2457),(#2458,
#2459),(#2460,#2461),(#2462,#2463),(#2464,#2465),(#2466,#2467),(#2468,#2469),
(#2470,#2471),(#2472,#2473),(#2474,#2475),(#2476,#2477),(#2478,#2479),(#2480,
#2481),(#2482,#2483),(#2484,#2485),(#2486,#2487),(#2488,#2489),(#2490,#2491),
(#2492,#2493),(#2494,#2495),(#2496,#2497),(#2498,#2499),(#2500,#2501)),
 .UNSPECIFIED.,.F.,.F.,.F.)
B_SPLINE_SURFACE_WITH_KNOTS((6,1,1,1,1,1,1,1,1,1,1,1,1,1,1,1,1,1,1,1,6),
(2,2),(0.,0.05,0.1,0.15,0.2,0.25,0.3,0.35,0.4,0.45,0.5,0.55,0.6,0.65,0.7,
0.75,0.8,0.85,0.9,0.95,1.),(0.,1.),.UNSPECIFIED.)
GEOMETRIC_REPRESENTATION_ITEM()
RATIONAL_B_SPLINE_SURFACE(((1.,1.),(1.,1.),(1.,1.),(1.,1.),(1.,1.),(1.,
1.),(1.,1.),(1.,1.),(1.,1.),(1.,1.),(1.,1.),(1.,1.),(1.,1.),(1.,1.),(1.,
1.),(1.,1.),(1.,1.),(1.,1.),(1.,1.),(1.,1.),(1.,1.),(1.,1.),(1.,1.),(1.,
1.),(1.,1.)))
REPRESENTATION_ITEM('')
SURFACE()
);
#68=SHAPE_REPRESENTATION_RELATIONSHIP('SRR','None',#4111,#76);
#69=SHAPE_REPRESENTATION_RELATIONSHIP('SRR','None',#4112,#77);
#70=SHAPE_REPRESENTATION_RELATIONSHIP('SRR','None',#4113,#78);
#71=SHAPE_REPRESENTATION_RELATIONSHIP('SRR','None',#4114,#79);
#72=SHAPE_REPRESENTATION_RELATIONSHIP('SRR','None',#4115,#80);
#73=SHAPE_REPRESENTATION_RELATIONSHIP('SRR','None',#4116,#81);
#74=SHAPE_REPRESENTATION_RELATIONSHIP('SRR','None',#4117,#82);
#75=SHAPE_REPRESENTATION_RELATIONSHIP('SRR','None',#4118,#83);
#76=ADVANCED_BREP_SHAPE_REPRESENTATION('',(#92),#4071);
#77=ADVANCED_BREP_SHAPE_REPRESENTATION('',(#93),#4072);
#78=ADVANCED_BREP_SHAPE_REPRESENTATION('',(#94),#4073);
#79=ADVANCED_BREP_SHAPE_REPRESENTATION('',(#95),#4074);
#80=ADVANCED_BREP_SHAPE_REPRESENTATION('',(#96),#4075);
#81=ADVANCED_BREP_SHAPE_REPRESENTATION('',(#97),#4076);
#82=ADVANCED_BREP_SHAPE_REPRESENTATION('',(#98),#4077);
#83=ADVANCED_BREP_SHAPE_REPRESENTATION('',(#99),#4078);
#84=STYLED_ITEM('',(#4160),#92);
#85=STYLED_ITEM('',(#4161),#93);
#86=STYLED_ITEM('',(#4162),#94);
#87=STYLED_ITEM('',(#4159),#95);
#88=STYLED_ITEM('',(#4159),#96);
#89=STYLED_ITEM('',(#4159),#97);
#90=STYLED_ITEM('',(#4159),#98);
#91=STYLED_ITEM('',(#4159),#99);
#92=MANIFOLD_SOLID_BREP('Wheel',#1443);
#93=MANIFOLD_SOLID_BREP('Pawl',#1444);
#94=MANIFOLD_SOLID_BREP('Spring',#1445);
#95=MANIFOLD_SOLID_BREP('Spacer',#1446);
#96=MANIFOLD_SOLID_BREP('Pin_02',#1447);
#97=MANIFOLD_SOLID_BREP('Spring_Holder',#1448);
#98=MANIFOLD_SOLID_BREP('Base',#1449);
#99=MANIFOLD_SOLID_BREP('Pin_01',#1450);
#100=FACE_BOUND('',#285,.T.);
#101=FACE_BOUND('',#308,.T.);
#102=FACE_BOUND('',#329,.T.);
#103=FACE_BOUND('',#331,.T.);
#104=FACE_BOUND('',#348,.T.);
#105=FACE_BOUND('',#350,.T.);
#106=CIRCLE('',#1544,37.4987147312734);
#107=CIRCLE('',#1545,37.4987147312734);
#108=CIRCLE('',#1548,37.4987147312734);
#109=CIRCLE('',#1549,37.4987147312734);
#110=CIRCLE('',#1550,37.4987147312734);
#111=CIRCLE('',#1551,37.4987147312734);
#112=CIRCLE('',#1552,37.4987147312734);
#113=CIRCLE('',#1553,37.4987147312734);
#114=CIRCLE('',#1554,37.4987147312734);
#115=CIRCLE('',#1555,37.4987147312735);
#116=CIRCLE('',#1556,37.4987147312734);
#117=CIRCLE('',#1557,37.4987147312734);
#118=CIRCLE('',#1558,37.4987147312734);
#119=CIRCLE('',#1559,37.4987147312734);
#120=CIRCLE('',#1560,37.4987147312734);
#121=CIRCLE('',#1561,37.4987147312734);
#122=CIRCLE('',#1562,37.4987147312734);
#123=CIRCLE('',#1563,37.4987147312734);
#124=CIRCLE('',#1564,37.4987147312734);
#125=CIRCLE('',#1565,14.4819556358054);
#126=CIRCLE('',#1568,37.4987147312734);
#127=CIRCLE('',#1572,37.4987147312734);
#128=CIRCLE('',#1575,37.4987147312734);
#129=CIRCLE('',#1577,37.4987147312734);
#130=CIRCLE('',#1579,37.4987147312734);
#131=CIRCLE('',#1582,37.4987147312734);
#132=CIRCLE('',#1585,37.4987147312734);
#133=CIRCLE('',#1587,37.4987147312734);
#134=CIRCLE('',#1589,37.4987147312734);
#135=CIRCLE('',#1592,37.4987147312734);
#136=CIRCLE('',#1595,37.4987147312734);
#137=CIRCLE('',#1598,37.4987147312735);
#138=CIRCLE('',#1600,37.4987147312734);
#139=CIRCLE('',#1601,37.4987147312734);
#140=CIRCLE('',#1602,37.4987147312734);
#141=CIRCLE('',#1603,37.4987147312734);
#142=CIRCLE('',#1604,37.4987147312734);
#143=CIRCLE('',#1605,14.4819556358054);
#144=CIRCLE('',#1621,6.);
#145=CIRCLE('',#1622,6.);
#146=CIRCLE('',#1624,10.6886401797172);
#147=CIRCLE('',#1625,10.6886401797172);
#148=CIRCLE('',#1627,37.4987147312738);
#149=CIRCLE('',#1628,37.4987147312738);
#150=CIRCLE('',#1633,1.);
#151=CIRCLE('',#1634,1.);
#152=CIRCLE('',#1635,1.);
#153=CIRCLE('',#1636,1.);
#154=CIRCLE('',#1637,1.);
#155=CIRCLE('',#1640,1.);
#156=CIRCLE('',#1641,1.);
#157=CIRCLE('',#1651,14.4819556358054);
#158=CIRCLE('',#1652,14.4819556358054);
#159=CIRCLE('',#1654,17.4819556358054);
#160=CIRCLE('',#1655,17.4819556358054);
#161=CIRCLE('',#1660,6.);
#162=CIRCLE('',#1661,6.);
#163=CIRCLE('',#1666,7.);
#164=CIRCLE('',#1667,7.);
#165=CIRCLE('',#1670,7.);
#166=CIRCLE('',#1672,7.);
#167=CIRCLE('',#1686,14.4819556358054);
#168=CIRCLE('',#1687,14.4819556358054);
#169=CYLINDRICAL_SURFACE('',#1543,37.4987147312734);
#170=CYLINDRICAL_SURFACE('',#1567,37.4987147312734);
#171=CYLINDRICAL_SURFACE('',#1571,37.4987147312734);
#172=CYLINDRICAL_SURFACE('',#1574,37.4987147312734);
#173=CYLINDRICAL_SURFACE('',#1576,37.4987147312734);
#174=CYLINDRICAL_SURFACE('',#1578,37.4987147312734);
#175=CYLINDRICAL_SURFACE('',#1581,37.4987147312734);
#176=CYLINDRICAL_SURFACE('',#1584,37.4987147312734);
#177=CYLINDRICAL_SURFACE('',#1586,37.4987147312734);
#178=CYLINDRICAL_SURFACE('',#1588,37.4987147312734);
#179=CYLINDRICAL_SURFACE('',#1591,37.4987147312734);
#180=CYLINDRICAL_SURFACE('',#1594,37.4987147312734);
#181=CYLINDRICAL_SURFACE('',#1597,37.4987147312735);
#182=CYLINDRICAL_SURFACE('',#1606,37.4987147312734);
#183=CYLINDRICAL_SURFACE('',#1608,37.4987147312734);
#184=CYLINDRICAL_SURFACE('',#1611,37.4987147312734);
#185=CYLINDRICAL_SURFACE('',#1613,37.4987147312734);
#186=CYLINDRICAL_SURFACE('',#1615,37.4987147312734);
#187=CYLINDRICAL_SURFACE('',#1618,14.4819556358054);
#188=CYLINDRICAL_SURFACE('',#1620,6.);
#189=CYLINDRICAL_SURFACE('',#1623,10.6886401797172);
#190=CYLINDRICAL_SURFACE('',#1626,37.4987147312738);
#191=CYLINDRICAL_SURFACE('',#1650,14.4819556358054);
#192=CYLINDRICAL_SURFACE('',#1653,17.4819556358054);
#193=CYLINDRICAL_SURFACE('',#1659,6.);
#194=CYLINDRICAL_SURFACE('',#1665,7.);
#195=CYLINDRICAL_SURFACE('',#1671,7.);
#196=CYLINDRICAL_SURFACE('',#1685,14.4819556358054);
#197=FACE_OUTER_BOUND('',#281,.T.);
#198=FACE_OUTER_BOUND('',#282,.T.);
#199=FACE_OUTER_BOUND('',#283,.T.);
#200=FACE_OUTER_BOUND('',#284,.T.);
#201=FACE_OUTER_BOUND('',#286,.T.);
#202=FACE_OUTER_BOUND('',#287,.T.);
#203=FACE_OUTER_BOUND('',#288,.T.);
#204=FACE_OUTER_BOUND('',#289,.T.);
#205=FACE_OUTER_BOUND('',#290,.T.);
#206=FACE_OUTER_BOUND('',#291,.T.);
#207=FACE_OUTER_BOUND('',#292,.T.);
#208=FACE_OUTER_BOUND('',#293,.T.);
#209=FACE_OUTER_BOUND('',#294,.T.);
#210=FACE_OUTER_BOUND('',#295,.T.);
#211=FACE_OUTER_BOUND('',#296,.T.);
#212=FACE_OUTER_BOUND('',#297,.T.);
#213=FACE_OUTER_BOUND('',#298,.T.);
#214=FACE_OUTER_BOUND('',#299,.T.);
#215=FACE_OUTER_BOUND('',#300,.T.);
#216=FACE_OUTER_BOUND('',#301,.T.);
#217=FACE_OUTER_BOUND('',#302,.T.);
#218=FACE_OUTER_BOUND('',#303,.T.);
#219=FACE_OUTER_BOUND('',#304,.T.);
#220=FACE_OUTER_BOUND('',#305,.T.);
#221=FACE_OUTER_BOUND('',#306,.T.);
#222=FACE_OUTER_BOUND('',#307,.T.);
#223=FACE_OUTER_BOUND('',#309,.T.);
#224=FACE_OUTER_BOUND('',#310,.T.);
#225=FACE_OUTER_BOUND('',#311,.T.);
#226=FACE_OUTER_BOUND('',#312,.T.);
#227=FACE_OUTER_BOUND('',#313,.T.);
#228=FACE_OUTER_BOUND('',#314,.T.);
#229=FACE_OUTER_BOUND('',#315,.T.);
#230=FACE_OUTER_BOUND('',#316,.T.);
#231=FACE_OUTER_BOUND('',#317,.T.);
#232=FACE_OUTER_BOUND('',#318,.T.);
#233=FACE_OUTER_BOUND('',#319,.T.);
#234=FACE_OUTER_BOUND('',#320,.T.);
#235=FACE_OUTER_BOUND('',#321,.T.);
#236=FACE_OUTER_BOUND('',#322,.T.);
#237=FACE_OUTER_BOUND('',#323,.T.);
#238=FACE_OUTER_BOUND('',#324,.T.);
#239=FACE_OUTER_BOUND('',#325,.T.);
#240=FACE_OUTER_BOUND('',#326,.T.);
#241=FACE_OUTER_BOUND('',#327,.T.);
#242=FACE_OUTER_BOUND('',#328,.T.);
#243=FACE_OUTER_BOUND('',#330,.T.);
#244=FACE_OUTER_BOUND('',#332,.T.);
#245=FACE_OUTER_BOUND('',#333,.T.);
#246=FACE_OUTER_BOUND('',#334,.T.);
#247=FACE_OUTER_BOUND('',#335,.T.);
#248=FACE_OUTER_BOUND('',#336,.T.);
#249=FACE_OUTER_BOUND('',#337,.T.);
#250=FACE_OUTER_BOUND('',#338,.T.);
#251=FACE_OUTER_BOUND('',#339,.T.);
#252=FACE_OUTER_BOUND('',#340,.T.);
#253=FACE_OUTER_BOUND('',#341,.T.);
#254=FACE_OUTER_BOUND('',#342,.T.);
#255=FACE_OUTER_BOUND('',#343,.T.);
#256=FACE_OUTER_BOUND('',#344,.T.);
#257=FACE_OUTER_BOUND('',#345,.T.);
#258=FACE_OUTER_BOUND('',#346,.T.);
#259=FACE_OUTER_BOUND('',#347,.T.);
#260=FACE_OUTER_BOUND('',#349,.T.);
#261=FACE_OUTER_BOUND('',#351,.T.);
#262=FACE_OUTER_BOUND('',#352,.T.);
#263=FACE_OUTER_BOUND('',#353,.T.);
#264=FACE_OUTER_BOUND('',#354,.T.);
#265=FACE_OUTER_BOUND('',#355,.T.);
#266=FACE_OUTER_BOUND('',#356,.T.);
#267=FACE_OUTER_BOUND('',#357,.T.);
#268=FACE_OUTER_BOUND('',#358,.T.);
#269=FACE_OUTER_BOUND('',#359,.T.);
#270=FACE_OUTER_BOUND('',#360,.T.);
#271=FACE_OUTER_BOUND('',#361,.T.);
#272=FACE_OUTER_BOUND('',#362,.T.);
#273=FACE_OUTER_BOUND('',#363,.T.);
#274=FACE_OUTER_BOUND('',#364,.T.);
#275=FACE_OUTER_BOUND('',#365,.T.);
#276=FACE_OUTER_BOUND('',#366,.T.);
#277=FACE_OUTER_BOUND('',#367,.T.);
#278=FACE_OUTER_BOUND('',#368,.T.);
#279=FACE_OUTER_BOUND('',#369,.T.);
#280=FACE_OUTER_BOUND('',#370,.T.);
#281=EDGE_LOOP('',(#919,#920,#921,#922));
#282=EDGE_LOOP('',(#923,#924,#925,#926));
#283=EDGE_LOOP('',(#927,#928,#929,#930));
#284=EDGE_LOOP('',(#931,#932,#933,#934,#935,#936,#937,#938,#939,#940,#941,
#942,#943,#944,#945,#946,#947,#948,#949,#950,#951,#952,#953,#954,#955,#956,
#957,#958,#959,#960,#961,#962,#963,#964,#965,#966));
#285=EDGE_LOOP('',(#967));
#286=EDGE_LOOP('',(#968,#969,#970,#971));
#287=EDGE_LOOP('',(#972,#973,#974,#975));
#288=EDGE_LOOP('',(#976,#977,#978,#979));
#289=EDGE_LOOP('',(#980,#981,#982,#983));
#290=EDGE_LOOP('',(#984,#985,#986,#987));
#291=EDGE_LOOP('',(#988,#989,#990,#991));
#292=EDGE_LOOP('',(#992,#993,#994,#995));
#293=EDGE_LOOP('',(#996,#997,#998,#999));
#294=EDGE_LOOP('',(#1000,#1001,#1002,#1003));
#295=EDGE_LOOP('',(#1004,#1005,#1006,#1007));
#296=EDGE_LOOP('',(#1008,#1009,#1010,#1011));
#297=EDGE_LOOP('',(#1012,#1013,#1014,#1015));
#298=EDGE_LOOP('',(#1016,#1017,#1018,#1019));
#299=EDGE_LOOP('',(#1020,#1021,#1022,#1023));
#300=EDGE_LOOP('',(#1024,#1025,#1026,#1027));
#301=EDGE_LOOP('',(#1028,#1029,#1030,#1031));
#302=EDGE_LOOP('',(#1032,#1033,#1034,#1035));
#303=EDGE_LOOP('',(#1036,#1037,#1038,#1039));
#304=EDGE_LOOP('',(#1040,#1041,#1042,#1043));
#305=EDGE_LOOP('',(#1044,#1045,#1046,#1047));
#306=EDGE_LOOP('',(#1048,#1049,#1050,#1051));
#307=EDGE_LOOP('',(#1052,#1053,#1054,#1055,#1056,#1057,#1058,#1059,#1060,
#1061,#1062,#1063,#1064,#1065,#1066,#1067,#1068,#1069,#1070,#1071,#1072,
#1073,#1074,#1075,#1076,#1077,#1078,#1079,#1080,#1081,#1082,#1083,#1084,
#1085,#1086,#1087));
#308=EDGE_LOOP('',(#1088));
#309=EDGE_LOOP('',(#1089,#1090,#1091,#1092));
#310=EDGE_LOOP('',(#1093,#1094,#1095,#1096));
#311=EDGE_LOOP('',(#1097,#1098,#1099,#1100));
#312=EDGE_LOOP('',(#1101,#1102,#1103,#1104));
#313=EDGE_LOOP('',(#1105,#1106,#1107,#1108));
#314=EDGE_LOOP('',(#1109,#1110,#1111,#1112));
#315=EDGE_LOOP('',(#1113,#1114,#1115,#1116));
#316=EDGE_LOOP('',(#1117,#1118,#1119,#1120));
#317=EDGE_LOOP('',(#1121,#1122,#1123,#1124));
#318=EDGE_LOOP('',(#1125,#1126,#1127,#1128));
#319=EDGE_LOOP('',(#1129,#1130,#1131,#1132));
#320=EDGE_LOOP('',(#1133,#1134,#1135,#1136));
#321=EDGE_LOOP('',(#1137,#1138,#1139,#1140));
#322=EDGE_LOOP('',(#1141,#1142,#1143,#1144));
#323=EDGE_LOOP('',(#1145,#1146,#1147,#1148));
#324=EDGE_LOOP('',(#1149,#1150,#1151,#1152));
#325=EDGE_LOOP('',(#1153,#1154,#1155,#1156));
#326=EDGE_LOOP('',(#1157,#1158,#1159,#1160));
#327=EDGE_LOOP('',(#1161,#1162,#1163,#1164));
#328=EDGE_LOOP('',(#1165,#1166,#1167,#1168,#1169));
#329=EDGE_LOOP('',(#1170));
#330=EDGE_LOOP('',(#1171,#1172,#1173,#1174,#1175));
#331=EDGE_LOOP('',(#1176));
#332=EDGE_LOOP('',(#1177,#1178,#1179,#1180,#1181,#1182,#1183,#1184,#1185));
#333=EDGE_LOOP('',(#1186,#1187,#1188,#1189,#1190,#1191,#1192,#1193,#1194));
#334=EDGE_LOOP('',(#1195,#1196,#1197));
#335=EDGE_LOOP('',(#1198,#1199,#1200));
#336=EDGE_LOOP('',(#1201,#1202,#1203,#1204,#1205,#1206,#1207));
#337=EDGE_LOOP('',(#1208,#1209,#1210));
#338=EDGE_LOOP('',(#1211,#1212));
#339=EDGE_LOOP('',(#1213,#1214));
#340=EDGE_LOOP('',(#1215));
#341=EDGE_LOOP('',(#1216,#1217,#1218,#1219));
#342=EDGE_LOOP('',(#1220,#1221));
#343=EDGE_LOOP('',(#1222));
#344=EDGE_LOOP('',(#1223,#1224));
#345=EDGE_LOOP('',(#1225,#1226,#1227,#1228));
#346=EDGE_LOOP('',(#1229,#1230,#1231,#1232));
#347=EDGE_LOOP('',(#1233));
#348=EDGE_LOOP('',(#1234));
#349=EDGE_LOOP('',(#1235));
#350=EDGE_LOOP('',(#1236));
#351=EDGE_LOOP('',(#1237,#1238,#1239,#1240));
#352=EDGE_LOOP('',(#1241));
#353=EDGE_LOOP('',(#1242));
#354=EDGE_LOOP('',(#1243,#1244,#1245,#1246));
#355=EDGE_LOOP('',(#1247,#1248,#1249,#1250));
#356=EDGE_LOOP('',(#1251,#1252,#1253,#1254,#1255,#1256));
#357=EDGE_LOOP('',(#1257,#1258,#1259,#1260));
#358=EDGE_LOOP('',(#1261,#1262,#1263,#1264,#1265,#1266));
#359=EDGE_LOOP('',(#1267,#1268,#1269,#1270));
#360=EDGE_LOOP('',(#1271,#1272,#1273,#1274));
#361=EDGE_LOOP('',(#1275,#1276,#1277,#1278));
#362=EDGE_LOOP('',(#1279,#1280,#1281,#1282));
#363=EDGE_LOOP('',(#1283,#1284,#1285,#1286));
#364=EDGE_LOOP('',(#1287,#1288,#1289,#1290));
#365=EDGE_LOOP('',(#1291,#1292,#1293,#1294));
#366=EDGE_LOOP('',(#1295,#1296,#1297,#1298));
#367=EDGE_LOOP('',(#1299,#1300,#1301,#1302));
#368=EDGE_LOOP('',(#1303,#1304,#1305,#1306));
#369=EDGE_LOOP('',(#1307));
#370=EDGE_LOOP('',(#1308));
#371=LINE('',#2132,#484);
#372=LINE('',#2134,#485);
#373=LINE('',#2136,#486);
#374=LINE('',#2137,#487);
#375=LINE('',#2141,#488);
#376=LINE('',#2146,#489);
#377=LINE('',#2148,#490);
#378=LINE('',#2149,#491);
#379=LINE('',#2154,#492);
#380=LINE('',#2158,#493);
#381=LINE('',#2162,#494);
#382=LINE('',#2166,#495);
#383=LINE('',#2170,#496);
#384=LINE('',#2174,#497);
#385=LINE('',#2178,#498);
#386=LINE('',#2182,#499);
#387=LINE('',#2186,#500);
#388=LINE('',#2190,#501);
#389=LINE('',#2194,#502);
#390=LINE('',#2198,#503);
#391=LINE('',#2202,#504);
#392=LINE('',#2206,#505);
#393=LINE('',#2210,#506);
#394=LINE('',#2214,#507);
#395=LINE('',#2220,#508);
#396=LINE('',#2222,#509);
#397=LINE('',#2223,#510);
#398=LINE('',#2226,#511);
#399=LINE('',#2230,#512);
#400=LINE('',#2231,#513);
#401=LINE('',#2234,#514);
#402=LINE('',#2236,#515);
#403=LINE('',#2237,#516);
#404=LINE('',#2240,#517);
#405=LINE('',#2244,#518);
#406=LINE('',#2245,#519);
#407=LINE('',#2250,#520);
#408=LINE('',#2255,#521);
#409=LINE('',#2257,#522);
#410=LINE('',#2260,#523);
#411=LINE('',#2263,#524);
#412=LINE('',#2266,#525);
#413=LINE('',#2267,#526);
#414=LINE('',#2271,#527);
#415=LINE('',#2274,#528);
#416=LINE('',#2279,#529);
#417=LINE('',#2281,#530);
#418=LINE('',#2284,#531);
#419=LINE('',#2287,#532);
#420=LINE('',#2290,#533);
#421=LINE('',#2291,#534);
#422=LINE('',#2294,#535);
#423=LINE('',#2297,#536);
#424=LINE('',#2300,#537);
#425=LINE('',#2301,#538);
#426=LINE('',#2305,#539);
#427=LINE('',#2308,#540);
#428=LINE('',#2312,#541);
#429=LINE('',#2316,#542);
#430=LINE('',#2319,#543);
#431=LINE('',#2321,#544);
#432=LINE('',#2325,#545);
#433=LINE('',#2327,#546);
#434=LINE('',#2331,#547);
#435=LINE('',#2332,#548);
#436=LINE('',#2335,#549);
#437=LINE('',#2338,#550);
#438=LINE('',#2339,#551);
#439=LINE('',#2341,#552);
#440=LINE('',#2344,#553);
#441=LINE('',#2345,#554);
#442=LINE('',#2348,#555);
#443=LINE('',#2352,#556);
#444=LINE('',#2358,#557);
#445=LINE('',#2423,#558);
#446=LINE('',#2445,#559);
#447=LINE('',#2451,#560);
#448=LINE('',#2554,#561);
#449=LINE('',#2560,#562);
#450=LINE('',#2562,#563);
#451=LINE('',#2563,#564);
#452=LINE('',#3599,#565);
#453=LINE('',#3949,#566);
#454=LINE('',#3958,#567);
#455=LINE('',#3964,#568);
#456=LINE('',#3973,#569);
#457=LINE('',#3983,#570);
#458=LINE('',#3986,#571);
#459=LINE('',#3989,#572);
#460=LINE('',#3991,#573);
#461=LINE('',#3992,#574);
#462=LINE('',#3995,#575);
#463=LINE('',#3997,#576);
#464=LINE('',#3999,#577);
#465=LINE('',#4004,#578);
#466=LINE('',#4007,#579);
#467=LINE('',#4009,#580);
#468=LINE('',#4010,#581);
#469=LINE('',#4012,#582);
#470=LINE('',#4014,#583);
#471=LINE('',#4020,#584);
#472=LINE('',#4022,#585);
#473=LINE('',#4024,#586);
#474=LINE('',#4025,#587);
#475=LINE('',#4028,#588);
#476=LINE('',#4030,#589);
#477=LINE('',#4031,#590);
#478=LINE('',#4034,#591);
#479=LINE('',#4036,#592);
#480=LINE('',#4037,#593);
#481=LINE('',#4039,#594);
#482=LINE('',#4040,#595);
#483=LINE('',#4048,#596);
#484=VECTOR('',#1704,10.);
#485=VECTOR('',#1705,10.);
#486=VECTOR('',#1706,10.);
#487=VECTOR('',#1707,10.);
#488=VECTOR('',#1710,10.);
#489=VECTOR('',#1717,10.);
#490=VECTOR('',#1718,10.);
#491=VECTOR('',#1719,10.);
#492=VECTOR('',#1724,10.);
#493=VECTOR('',#1727,10.);
#494=VECTOR('',#1730,10.);
#495=VECTOR('',#1733,10.);
#496=VECTOR('',#1736,10.);
#497=VECTOR('',#1739,10.);
#498=VECTOR('',#1742,10.);
#499=VECTOR('',#1745,10.);
#500=VECTOR('',#1748,10.);
#501=VECTOR('',#1751,10.);
#502=VECTOR('',#1754,10.);
#503=VECTOR('',#1757,10.);
#504=VECTOR('',#1760,10.);
#505=VECTOR('',#1763,10.);
#506=VECTOR('',#1766,10.);
#507=VECTOR('',#1769,10.);
#508=VECTOR('',#1776,10.);
#509=VECTOR('',#1777,10.);
#510=VECTOR('',#1778,10.);
#511=VECTOR('',#1781,10.);
#512=VECTOR('',#1786,10.);
#513=VECTOR('',#1787,10.);
#514=VECTOR('',#1790,10.);
#515=VECTOR('',#1791,10.);
#516=VECTOR('',#1792,10.);
#517=VECTOR('',#1795,10.);
#518=VECTOR('',#1800,10.);
#519=VECTOR('',#1801,10.);
#520=VECTOR('',#1808,10.);
#521=VECTOR('',#1815,10.);
#522=VECTOR('',#1818,10.);
#523=VECTOR('',#1821,10.);
#524=VECTOR('',#1824,10.);
#525=VECTOR('',#1827,10.);
#526=VECTOR('',#1828,10.);
#527=VECTOR('',#1833,10.);
#528=VECTOR('',#1836,10.);
#529=VECTOR('',#1843,10.);
#530=VECTOR('',#1846,10.);
#531=VECTOR('',#1849,10.);
#532=VECTOR('',#1852,10.);
#533=VECTOR('',#1855,10.);
#534=VECTOR('',#1856,10.);
#535=VECTOR('',#1859,10.);
#536=VECTOR('',#1862,10.);
#537=VECTOR('',#1865,10.);
#538=VECTOR('',#1866,10.);
#539=VECTOR('',#1871,10.);
#540=VECTOR('',#1874,10.);
#541=VECTOR('',#1877,10.);
#542=VECTOR('',#1880,10.);
#543=VECTOR('',#1883,10.);
#544=VECTOR('',#1884,10.);
#545=VECTOR('',#1887,10.);
#546=VECTOR('',#1890,10.);
#547=VECTOR('',#1895,10.);
#548=VECTOR('',#1896,10.);
#549=VECTOR('',#1901,10.);
#550=VECTOR('',#1906,10.);
#551=VECTOR('',#1907,10.);
#552=VECTOR('',#1910,10.);
#553=VECTOR('',#1915,10.);
#554=VECTOR('',#1916,10.);
#555=VECTOR('',#1921,10.);
#556=VECTOR('',#1928,14.4819556358054);
#557=VECTOR('',#1935,6.);
#558=VECTOR('',#1938,10.);
#559=VECTOR('',#1939,10.);
#560=VECTOR('',#1946,10.);
#561=VECTOR('',#1947,10.);
#562=VECTOR('',#1954,10.);
#563=VECTOR('',#1957,10.);
#564=VECTOR('',#1958,10.);
#565=VECTOR('',#1979,10.);
#566=VECTOR('',#1992,10.);
#567=VECTOR('',#2005,14.4819556358054);
#568=VECTOR('',#2012,17.4819556358054);
#569=VECTOR('',#2025,6.);
#570=VECTOR('',#2038,10.);
#571=VECTOR('',#2041,10.);
#572=VECTOR('',#2044,10.);
#573=VECTOR('',#2045,10.);
#574=VECTOR('',#2046,10.);
#575=VECTOR('',#2049,10.);
#576=VECTOR('',#2050,10.);
#577=VECTOR('',#2051,10.);
#578=VECTOR('',#2058,10.);
#579=VECTOR('',#2061,10.);
#580=VECTOR('',#2062,10.);
#581=VECTOR('',#2063,10.);
#582=VECTOR('',#2066,10.);
#583=VECTOR('',#2069,10.);
#584=VECTOR('',#2076,10.);
#585=VECTOR('',#2077,10.);
#586=VECTOR('',#2078,10.);
#587=VECTOR('',#2079,10.);
#588=VECTOR('',#2082,10.);
#589=VECTOR('',#2083,10.);
#590=VECTOR('',#2084,10.);
#591=VECTOR('',#2087,10.);
#592=VECTOR('',#2088,10.);
#593=VECTOR('',#2089,10.);
#594=VECTOR('',#2092,10.);
#595=VECTOR('',#2093,10.);
#596=VECTOR('',#2104,14.4819556358054);
#597=VERTEX_POINT('',#2130);
#598=VERTEX_POINT('',#2131);
#599=VERTEX_POINT('',#2133);
#600=VERTEX_POINT('',#2135);
#601=VERTEX_POINT('',#2139);
#602=VERTEX_POINT('',#2140);
#603=VERTEX_POINT('',#2145);
#604=VERTEX_POINT('',#2147);
#605=VERTEX_POINT('',#2151);
#606=VERTEX_POINT('',#2153);
#607=VERTEX_POINT('',#2155);
#608=VERTEX_POINT('',#2157);
#609=VERTEX_POINT('',#2159);
#610=VERTEX_POINT('',#2161);
#611=VERTEX_POINT('',#2163);
#612=VERTEX_POINT('',#2165);
#613=VERTEX_POINT('',#2167);
#614=VERTEX_POINT('',#2169);
#615=VERTEX_POINT('',#2171);
#616=VERTEX_POINT('',#2173);
#617=VERTEX_POINT('',#2175);
#618=VERTEX_POINT('',#2177);
#619=VERTEX_POINT('',#2179);
#620=VERTEX_POINT('',#2181);
#621=VERTEX_POINT('',#2183);
#622=VERTEX_POINT('',#2185);
#623=VERTEX_POINT('',#2187);
#624=VERTEX_POINT('',#2189);
#625=VERTEX_POINT('',#2191);
#626=VERTEX_POINT('',#2193);
#627=VERTEX_POINT('',#2195);
#628=VERTEX_POINT('',#2197);
#629=VERTEX_POINT('',#2199);
#630=VERTEX_POINT('',#2201);
#631=VERTEX_POINT('',#2203);
#632=VERTEX_POINT('',#2205);
#633=VERTEX_POINT('',#2207);
#634=VERTEX_POINT('',#2209);
#635=VERTEX_POINT('',#2211);
#636=VERTEX_POINT('',#2213);
#637=VERTEX_POINT('',#2216);
#638=VERTEX_POINT('',#2219);
#639=VERTEX_POINT('',#2221);
#640=VERTEX_POINT('',#2225);
#641=VERTEX_POINT('',#2229);
#642=VERTEX_POINT('',#2233);
#643=VERTEX_POINT('',#2235);
#644=VERTEX_POINT('',#2239);
#645=VERTEX_POINT('',#2243);
#646=VERTEX_POINT('',#2249);
#647=VERTEX_POINT('',#2253);
#648=VERTEX_POINT('',#2259);
#649=VERTEX_POINT('',#2261);
#650=VERTEX_POINT('',#2265);
#651=VERTEX_POINT('',#2269);
#652=VERTEX_POINT('',#2273);
#653=VERTEX_POINT('',#2277);
#654=VERTEX_POINT('',#2283);
#655=VERTEX_POINT('',#2285);
#656=VERTEX_POINT('',#2289);
#657=VERTEX_POINT('',#2293);
#658=VERTEX_POINT('',#2295);
#659=VERTEX_POINT('',#2299);
#660=VERTEX_POINT('',#2303);
#661=VERTEX_POINT('',#2307);
#662=VERTEX_POINT('',#2309);
#663=VERTEX_POINT('',#2311);
#664=VERTEX_POINT('',#2313);
#665=VERTEX_POINT('',#2315);
#666=VERTEX_POINT('',#2317);
#667=VERTEX_POINT('',#2320);
#668=VERTEX_POINT('',#2322);
#669=VERTEX_POINT('',#2324);
#670=VERTEX_POINT('',#2328);
#671=VERTEX_POINT('',#2355);
#672=VERTEX_POINT('',#2357);
#673=VERTEX_POINT('',#2400);
#674=VERTEX_POINT('',#2401);
#675=VERTEX_POINT('',#2422);
#676=VERTEX_POINT('',#2424);
#677=VERTEX_POINT('',#2447);
#678=VERTEX_POINT('',#2449);
#679=VERTEX_POINT('',#2502);
#680=VERTEX_POINT('',#2528);
#681=VERTEX_POINT('',#2556);
#682=VERTEX_POINT('',#2558);
#683=VERTEX_POINT('',#2657);
#684=VERTEX_POINT('',#2658);
#685=VERTEX_POINT('',#2687);
#686=VERTEX_POINT('',#2698);
#687=VERTEX_POINT('',#2701);
#688=VERTEX_POINT('',#2722);
#689=VERTEX_POINT('',#3426);
#690=VERTEX_POINT('',#3494);
#691=VERTEX_POINT('',#3515);
#692=VERTEX_POINT('',#3532);
#693=VERTEX_POINT('',#3539);
#694=VERTEX_POINT('',#3598);
#695=VERTEX_POINT('',#3899);
#696=VERTEX_POINT('',#3955);
#697=VERTEX_POINT('',#3957);
#698=VERTEX_POINT('',#3961);
#699=VERTEX_POINT('',#3963);
#700=VERTEX_POINT('',#3970);
#701=VERTEX_POINT('',#3972);
#702=VERTEX_POINT('',#3979);
#703=VERTEX_POINT('',#3980);
#704=VERTEX_POINT('',#3982);
#705=VERTEX_POINT('',#3984);
#706=VERTEX_POINT('',#3988);
#707=VERTEX_POINT('',#3990);
#708=VERTEX_POINT('',#3994);
#709=VERTEX_POINT('',#3996);
#710=VERTEX_POINT('',#3998);
#711=VERTEX_POINT('',#4002);
#712=VERTEX_POINT('',#4006);
#713=VERTEX_POINT('',#4008);
#714=VERTEX_POINT('',#4018);
#715=VERTEX_POINT('',#4019);
#716=VERTEX_POINT('',#4021);
#717=VERTEX_POINT('',#4023);
#718=VERTEX_POINT('',#4027);
#719=VERTEX_POINT('',#4029);
#720=VERTEX_POINT('',#4033);
#721=VERTEX_POINT('',#4035);
#722=VERTEX_POINT('',#4045);
#723=VERTEX_POINT('',#4047);
#724=EDGE_CURVE('',#597,#598,#371,.T.);
#725=EDGE_CURVE('',#597,#599,#372,.T.);
#726=EDGE_CURVE('',#599,#600,#373,.T.);
#727=EDGE_CURVE('',#598,#600,#374,.T.);
#728=EDGE_CURVE('',#601,#602,#375,.T.);
#729=EDGE_CURVE('',#600,#601,#106,.T.);
#730=EDGE_CURVE('',#602,#599,#107,.T.);
#731=EDGE_CURVE('',#602,#603,#376,.T.);
#732=EDGE_CURVE('',#603,#604,#377,.T.);
#733=EDGE_CURVE('',#601,#604,#378,.T.);
#734=EDGE_CURVE('',#597,#605,#108,.T.);
#735=EDGE_CURVE('',#606,#605,#379,.T.);
#736=EDGE_CURVE('',#606,#607,#109,.T.);
#737=EDGE_CURVE('',#608,#607,#380,.T.);
#738=EDGE_CURVE('',#608,#609,#110,.T.);
#739=EDGE_CURVE('',#610,#609,#381,.T.);
#740=EDGE_CURVE('',#610,#611,#111,.T.);
#741=EDGE_CURVE('',#612,#611,#382,.T.);
#742=EDGE_CURVE('',#612,#613,#112,.T.);
#743=EDGE_CURVE('',#614,#613,#383,.T.);
#744=EDGE_CURVE('',#614,#615,#113,.T.);
#745=EDGE_CURVE('',#616,#615,#384,.T.);
#746=EDGE_CURVE('',#616,#617,#114,.T.);
#747=EDGE_CURVE('',#618,#617,#385,.T.);
#748=EDGE_CURVE('',#618,#619,#115,.T.);
#749=EDGE_CURVE('',#620,#619,#386,.T.);
#750=EDGE_CURVE('',#620,#621,#116,.T.);
#751=EDGE_CURVE('',#622,#621,#387,.T.);
#752=EDGE_CURVE('',#622,#623,#117,.T.);
#753=EDGE_CURVE('',#624,#623,#388,.T.);
#754=EDGE_CURVE('',#624,#625,#118,.T.);
#755=EDGE_CURVE('',#626,#625,#389,.T.);
#756=EDGE_CURVE('',#626,#627,#119,.T.);
#757=EDGE_CURVE('',#628,#627,#390,.T.);
#758=EDGE_CURVE('',#628,#629,#120,.T.);
#759=EDGE_CURVE('',#630,#629,#391,.T.);
#760=EDGE_CURVE('',#630,#631,#121,.T.);
#761=EDGE_CURVE('',#632,#631,#392,.T.);
#762=EDGE_CURVE('',#632,#633,#122,.T.);
#763=EDGE_CURVE('',#634,#633,#393,.T.);
#764=EDGE_CURVE('',#634,#635,#123,.T.);
#765=EDGE_CURVE('',#636,#635,#394,.T.);
#766=EDGE_CURVE('',#636,#603,#124,.T.);
#767=EDGE_CURVE('',#637,#637,#125,.T.);
#768=EDGE_CURVE('',#636,#638,#395,.T.);
#769=EDGE_CURVE('',#635,#639,#396,.T.);
#770=EDGE_CURVE('',#638,#639,#397,.T.);
#771=EDGE_CURVE('',#640,#634,#398,.T.);
#772=EDGE_CURVE('',#639,#640,#126,.T.);
#773=EDGE_CURVE('',#633,#641,#399,.T.);
#774=EDGE_CURVE('',#640,#641,#400,.T.);
#775=EDGE_CURVE('',#630,#642,#401,.T.);
#776=EDGE_CURVE('',#629,#643,#402,.T.);
#777=EDGE_CURVE('',#642,#643,#403,.T.);
#778=EDGE_CURVE('',#644,#628,#404,.T.);
#779=EDGE_CURVE('',#643,#644,#127,.T.);
#780=EDGE_CURVE('',#627,#645,#405,.T.);
#781=EDGE_CURVE('',#644,#645,#406,.T.);
#782=EDGE_CURVE('',#604,#638,#128,.T.);
#783=EDGE_CURVE('',#646,#632,#407,.T.);
#784=EDGE_CURVE('',#641,#646,#129,.T.);
#785=EDGE_CURVE('',#647,#642,#130,.T.);
#786=EDGE_CURVE('',#631,#647,#408,.T.);
#787=EDGE_CURVE('',#646,#647,#409,.T.);
#788=EDGE_CURVE('',#648,#606,#410,.T.);
#789=EDGE_CURVE('',#649,#648,#131,.T.);
#790=EDGE_CURVE('',#607,#649,#411,.T.);
#791=EDGE_CURVE('',#608,#650,#412,.T.);
#792=EDGE_CURVE('',#650,#649,#413,.T.);
#793=EDGE_CURVE('',#651,#650,#132,.T.);
#794=EDGE_CURVE('',#609,#651,#414,.T.);
#795=EDGE_CURVE('',#652,#626,#415,.T.);
#796=EDGE_CURVE('',#645,#652,#133,.T.);
#797=EDGE_CURVE('',#653,#598,#134,.T.);
#798=EDGE_CURVE('',#605,#653,#416,.T.);
#799=EDGE_CURVE('',#648,#653,#417,.T.);
#800=EDGE_CURVE('',#654,#610,#418,.T.);
#801=EDGE_CURVE('',#655,#654,#135,.T.);
#802=EDGE_CURVE('',#611,#655,#419,.T.);
#803=EDGE_CURVE('',#612,#656,#420,.T.);
#804=EDGE_CURVE('',#656,#655,#421,.T.);
#805=EDGE_CURVE('',#657,#616,#422,.T.);
#806=EDGE_CURVE('',#658,#657,#136,.T.);
#807=EDGE_CURVE('',#617,#658,#423,.T.);
#808=EDGE_CURVE('',#618,#659,#424,.T.);
#809=EDGE_CURVE('',#659,#658,#425,.T.);
#810=EDGE_CURVE('',#660,#659,#137,.T.);
#811=EDGE_CURVE('',#619,#660,#426,.T.);
#812=EDGE_CURVE('',#652,#661,#427,.T.);
#813=EDGE_CURVE('',#661,#662,#138,.T.);
#814=EDGE_CURVE('',#662,#663,#428,.T.);
#815=EDGE_CURVE('',#663,#664,#139,.T.);
#816=EDGE_CURVE('',#664,#665,#429,.T.);
#817=EDGE_CURVE('',#665,#666,#140,.T.);
#818=EDGE_CURVE('',#666,#660,#430,.T.);
#819=EDGE_CURVE('',#657,#667,#431,.T.);
#820=EDGE_CURVE('',#667,#668,#141,.T.);
#821=EDGE_CURVE('',#668,#669,#432,.T.);
#822=EDGE_CURVE('',#669,#656,#142,.T.);
#823=EDGE_CURVE('',#654,#651,#433,.T.);
#824=EDGE_CURVE('',#670,#670,#143,.T.);
#825=EDGE_CURVE('',#668,#614,#434,.T.);
#826=EDGE_CURVE('',#615,#667,#435,.T.);
#827=EDGE_CURVE('',#613,#669,#436,.T.);
#828=EDGE_CURVE('',#622,#664,#437,.T.);
#829=EDGE_CURVE('',#621,#665,#438,.T.);
#830=EDGE_CURVE('',#666,#620,#439,.T.);
#831=EDGE_CURVE('',#662,#624,#440,.T.);
#832=EDGE_CURVE('',#625,#661,#441,.T.);
#833=EDGE_CURVE('',#623,#663,#442,.T.);
#834=EDGE_CURVE('',#670,#637,#443,.T.);
#835=EDGE_CURVE('',#671,#671,#144,.T.);
#836=EDGE_CURVE('',#671,#672,#444,.T.);
#837=EDGE_CURVE('',#672,#672,#145,.T.);
#838=EDGE_CURVE('',#673,#674,#62,.T.);
#839=EDGE_CURVE('',#673,#675,#445,.T.);
#840=EDGE_CURVE('',#676,#675,#63,.T.);
#841=EDGE_CURVE('',#674,#676,#446,.T.);
#842=EDGE_CURVE('',#674,#677,#146,.T.);
#843=EDGE_CURVE('',#678,#676,#147,.T.);
#844=EDGE_CURVE('',#677,#678,#447,.T.);
#845=EDGE_CURVE('',#679,#677,#64,.T.);
#846=EDGE_CURVE('',#680,#678,#65,.T.);
#847=EDGE_CURVE('',#679,#680,#448,.T.);
#848=EDGE_CURVE('',#681,#679,#148,.T.);
#849=EDGE_CURVE('',#682,#680,#149,.T.);
#850=EDGE_CURVE('',#681,#682,#449,.T.);
#851=EDGE_CURVE('',#681,#673,#450,.T.);
#852=EDGE_CURVE('',#675,#682,#451,.T.);
#853=EDGE_CURVE('',#683,#684,#43,.T.);
#854=EDGE_CURVE('',#684,#685,#44,.T.);
#855=EDGE_CURVE('',#685,#686,#150,.T.);
#856=EDGE_CURVE('',#686,#685,#151,.T.);
#857=EDGE_CURVE('',#685,#687,#45,.T.);
#858=EDGE_CURVE('',#687,#683,#46,.T.);
#859=EDGE_CURVE('',#683,#688,#47,.T.);
#860=EDGE_CURVE('',#688,#688,#152,.T.);
#861=EDGE_CURVE('',#686,#685,#48,.T.);
#862=EDGE_CURVE('',#686,#689,#49,.T.);
#863=EDGE_CURVE('',#689,#690,#50,.T.);
#864=EDGE_CURVE('',#690,#691,#51,.T.);
#865=EDGE_CURVE('',#691,#692,#52,.T.);
#866=EDGE_CURVE('',#693,#692,#153,.T.);
#867=EDGE_CURVE('',#693,#689,#154,.T.);
#868=EDGE_CURVE('',#686,#685,#53,.T.);
#869=EDGE_CURVE('',#684,#687,#54,.T.);
#870=EDGE_CURVE('',#693,#694,#452,.T.);
#871=EDGE_CURVE('',#694,#689,#55,.T.);
#872=EDGE_CURVE('',#691,#694,#56,.T.);
#873=EDGE_CURVE('',#690,#689,#155,.T.);
#874=EDGE_CURVE('',#689,#695,#57,.T.);
#875=EDGE_CURVE('',#695,#695,#156,.T.);
#876=EDGE_CURVE('',#692,#693,#453,.F.);
#877=EDGE_CURVE('',#696,#696,#157,.T.);
#878=EDGE_CURVE('',#696,#697,#454,.T.);
#879=EDGE_CURVE('',#697,#697,#158,.T.);
#880=EDGE_CURVE('',#698,#698,#159,.T.);
#881=EDGE_CURVE('',#698,#699,#455,.T.);
#882=EDGE_CURVE('',#699,#699,#160,.T.);
#883=EDGE_CURVE('',#700,#700,#161,.T.);
#884=EDGE_CURVE('',#700,#701,#456,.T.);
#885=EDGE_CURVE('',#701,#701,#162,.T.);
#886=EDGE_CURVE('',#702,#703,#163,.T.);
#887=EDGE_CURVE('',#703,#704,#457,.T.);
#888=EDGE_CURVE('',#704,#705,#164,.T.);
#889=EDGE_CURVE('',#705,#702,#458,.T.);
#890=EDGE_CURVE('',#703,#706,#459,.T.);
#891=EDGE_CURVE('',#707,#706,#460,.T.);
#892=EDGE_CURVE('',#707,#704,#461,.T.);
#893=EDGE_CURVE('',#708,#702,#462,.T.);
#894=EDGE_CURVE('',#709,#708,#463,.T.);
#895=EDGE_CURVE('',#709,#710,#464,.T.);
#896=EDGE_CURVE('',#706,#710,#165,.T.);
#897=EDGE_CURVE('',#711,#707,#166,.T.);
#898=EDGE_CURVE('',#710,#711,#465,.T.);
#899=EDGE_CURVE('',#712,#711,#466,.T.);
#900=EDGE_CURVE('',#713,#712,#467,.T.);
#901=EDGE_CURVE('',#713,#705,#468,.T.);
#902=EDGE_CURVE('',#712,#709,#469,.T.);
#903=EDGE_CURVE('',#708,#713,#470,.T.);
#904=EDGE_CURVE('',#714,#715,#471,.T.);
#905=EDGE_CURVE('',#714,#716,#472,.T.);
#906=EDGE_CURVE('',#717,#716,#473,.T.);
#907=EDGE_CURVE('',#715,#717,#474,.T.);
#908=EDGE_CURVE('',#715,#718,#475,.T.);
#909=EDGE_CURVE('',#719,#717,#476,.T.);
#910=EDGE_CURVE('',#718,#719,#477,.T.);
#911=EDGE_CURVE('',#718,#720,#478,.T.);
#912=EDGE_CURVE('',#721,#719,#479,.T.);
#913=EDGE_CURVE('',#720,#721,#480,.T.);
#914=EDGE_CURVE('',#720,#714,#481,.T.);
#915=EDGE_CURVE('',#716,#721,#482,.T.);
#916=EDGE_CURVE('',#722,#722,#167,.T.);
#917=EDGE_CURVE('',#722,#723,#483,.T.);
#918=EDGE_CURVE('',#723,#723,#168,.T.);
#919=ORIENTED_EDGE('',*,*,#724,.F.);
#920=ORIENTED_EDGE('',*,*,#725,.T.);
#921=ORIENTED_EDGE('',*,*,#726,.T.);
#922=ORIENTED_EDGE('',*,*,#727,.F.);
#923=ORIENTED_EDGE('',*,*,#728,.F.);
#924=ORIENTED_EDGE('',*,*,#729,.F.);
#925=ORIENTED_EDGE('',*,*,#726,.F.);
#926=ORIENTED_EDGE('',*,*,#730,.F.);
#927=ORIENTED_EDGE('',*,*,#728,.T.);
#928=ORIENTED_EDGE('',*,*,#731,.T.);
#929=ORIENTED_EDGE('',*,*,#732,.T.);
#930=ORIENTED_EDGE('',*,*,#733,.F.);
#931=ORIENTED_EDGE('',*,*,#730,.T.);
#932=ORIENTED_EDGE('',*,*,#725,.F.);
#933=ORIENTED_EDGE('',*,*,#734,.T.);
#934=ORIENTED_EDGE('',*,*,#735,.F.);
#935=ORIENTED_EDGE('',*,*,#736,.T.);
#936=ORIENTED_EDGE('',*,*,#737,.F.);
#937=ORIENTED_EDGE('',*,*,#738,.T.);
#938=ORIENTED_EDGE('',*,*,#739,.F.);
#939=ORIENTED_EDGE('',*,*,#740,.T.);
#940=ORIENTED_EDGE('',*,*,#741,.F.);
#941=ORIENTED_EDGE('',*,*,#742,.T.);
#942=ORIENTED_EDGE('',*,*,#743,.F.);
#943=ORIENTED_EDGE('',*,*,#744,.T.);
#944=ORIENTED_EDGE('',*,*,#745,.F.);
#945=ORIENTED_EDGE('',*,*,#746,.T.);
#946=ORIENTED_EDGE('',*,*,#747,.F.);
#947=ORIENTED_EDGE('',*,*,#748,.T.);
#948=ORIENTED_EDGE('',*,*,#749,.F.);
#949=ORIENTED_EDGE('',*,*,#750,.T.);
#950=ORIENTED_EDGE('',*,*,#751,.F.);
#951=ORIENTED_EDGE('',*,*,#752,.T.);
#952=ORIENTED_EDGE('',*,*,#753,.F.);
#953=ORIENTED_EDGE('',*,*,#754,.T.);
#954=ORIENTED_EDGE('',*,*,#755,.F.);
#955=ORIENTED_EDGE('',*,*,#756,.T.);
#956=ORIENTED_EDGE('',*,*,#757,.F.);
#957=ORIENTED_EDGE('',*,*,#758,.T.);
#958=ORIENTED_EDGE('',*,*,#759,.F.);
#959=ORIENTED_EDGE('',*,*,#760,.T.);
#960=ORIENTED_EDGE('',*,*,#761,.F.);
#961=ORIENTED_EDGE('',*,*,#762,.T.);
#962=ORIENTED_EDGE('',*,*,#763,.F.);
#963=ORIENTED_EDGE('',*,*,#764,.T.);
#964=ORIENTED_EDGE('',*,*,#765,.F.);
#965=ORIENTED_EDGE('',*,*,#766,.T.);
#966=ORIENTED_EDGE('',*,*,#731,.F.);
#967=ORIENTED_EDGE('',*,*,#767,.T.);
#968=ORIENTED_EDGE('',*,*,#768,.F.);
#969=ORIENTED_EDGE('',*,*,#765,.T.);
#970=ORIENTED_EDGE('',*,*,#769,.T.);
#971=ORIENTED_EDGE('',*,*,#770,.F.);
#972=ORIENTED_EDGE('',*,*,#771,.F.);
#973=ORIENTED_EDGE('',*,*,#772,.F.);
#974=ORIENTED_EDGE('',*,*,#769,.F.);
#975=ORIENTED_EDGE('',*,*,#764,.F.);
#976=ORIENTED_EDGE('',*,*,#771,.T.);
#977=ORIENTED_EDGE('',*,*,#763,.T.);
#978=ORIENTED_EDGE('',*,*,#773,.T.);
#979=ORIENTED_EDGE('',*,*,#774,.F.);
#980=ORIENTED_EDGE('',*,*,#775,.F.);
#981=ORIENTED_EDGE('',*,*,#759,.T.);
#982=ORIENTED_EDGE('',*,*,#776,.T.);
#983=ORIENTED_EDGE('',*,*,#777,.F.);
#984=ORIENTED_EDGE('',*,*,#778,.F.);
#985=ORIENTED_EDGE('',*,*,#779,.F.);
#986=ORIENTED_EDGE('',*,*,#776,.F.);
#987=ORIENTED_EDGE('',*,*,#758,.F.);
#988=ORIENTED_EDGE('',*,*,#778,.T.);
#989=ORIENTED_EDGE('',*,*,#757,.T.);
#990=ORIENTED_EDGE('',*,*,#780,.T.);
#991=ORIENTED_EDGE('',*,*,#781,.F.);
#992=ORIENTED_EDGE('',*,*,#768,.T.);
#993=ORIENTED_EDGE('',*,*,#782,.F.);
#994=ORIENTED_EDGE('',*,*,#732,.F.);
#995=ORIENTED_EDGE('',*,*,#766,.F.);
#996=ORIENTED_EDGE('',*,*,#783,.F.);
#997=ORIENTED_EDGE('',*,*,#784,.F.);
#998=ORIENTED_EDGE('',*,*,#773,.F.);
#999=ORIENTED_EDGE('',*,*,#762,.F.);
#1000=ORIENTED_EDGE('',*,*,#775,.T.);
#1001=ORIENTED_EDGE('',*,*,#785,.F.);
#1002=ORIENTED_EDGE('',*,*,#786,.F.);
#1003=ORIENTED_EDGE('',*,*,#760,.F.);
#1004=ORIENTED_EDGE('',*,*,#783,.T.);
#1005=ORIENTED_EDGE('',*,*,#761,.T.);
#1006=ORIENTED_EDGE('',*,*,#786,.T.);
#1007=ORIENTED_EDGE('',*,*,#787,.F.);
#1008=ORIENTED_EDGE('',*,*,#788,.F.);
#1009=ORIENTED_EDGE('',*,*,#789,.F.);
#1010=ORIENTED_EDGE('',*,*,#790,.F.);
#1011=ORIENTED_EDGE('',*,*,#736,.F.);
#1012=ORIENTED_EDGE('',*,*,#791,.F.);
#1013=ORIENTED_EDGE('',*,*,#737,.T.);
#1014=ORIENTED_EDGE('',*,*,#790,.T.);
#1015=ORIENTED_EDGE('',*,*,#792,.F.);
#1016=ORIENTED_EDGE('',*,*,#791,.T.);
#1017=ORIENTED_EDGE('',*,*,#793,.F.);
#1018=ORIENTED_EDGE('',*,*,#794,.F.);
#1019=ORIENTED_EDGE('',*,*,#738,.F.);
#1020=ORIENTED_EDGE('',*,*,#795,.F.);
#1021=ORIENTED_EDGE('',*,*,#796,.F.);
#1022=ORIENTED_EDGE('',*,*,#780,.F.);
#1023=ORIENTED_EDGE('',*,*,#756,.F.);
#1024=ORIENTED_EDGE('',*,*,#724,.T.);
#1025=ORIENTED_EDGE('',*,*,#797,.F.);
#1026=ORIENTED_EDGE('',*,*,#798,.F.);
#1027=ORIENTED_EDGE('',*,*,#734,.F.);
#1028=ORIENTED_EDGE('',*,*,#788,.T.);
#1029=ORIENTED_EDGE('',*,*,#735,.T.);
#1030=ORIENTED_EDGE('',*,*,#798,.T.);
#1031=ORIENTED_EDGE('',*,*,#799,.F.);
#1032=ORIENTED_EDGE('',*,*,#800,.F.);
#1033=ORIENTED_EDGE('',*,*,#801,.F.);
#1034=ORIENTED_EDGE('',*,*,#802,.F.);
#1035=ORIENTED_EDGE('',*,*,#740,.F.);
#1036=ORIENTED_EDGE('',*,*,#803,.F.);
#1037=ORIENTED_EDGE('',*,*,#741,.T.);
#1038=ORIENTED_EDGE('',*,*,#802,.T.);
#1039=ORIENTED_EDGE('',*,*,#804,.F.);
#1040=ORIENTED_EDGE('',*,*,#805,.F.);
#1041=ORIENTED_EDGE('',*,*,#806,.F.);
#1042=ORIENTED_EDGE('',*,*,#807,.F.);
#1043=ORIENTED_EDGE('',*,*,#746,.F.);
#1044=ORIENTED_EDGE('',*,*,#808,.F.);
#1045=ORIENTED_EDGE('',*,*,#747,.T.);
#1046=ORIENTED_EDGE('',*,*,#807,.T.);
#1047=ORIENTED_EDGE('',*,*,#809,.F.);
#1048=ORIENTED_EDGE('',*,*,#808,.T.);
#1049=ORIENTED_EDGE('',*,*,#810,.F.);
#1050=ORIENTED_EDGE('',*,*,#811,.F.);
#1051=ORIENTED_EDGE('',*,*,#748,.F.);
#1052=ORIENTED_EDGE('',*,*,#733,.T.);
#1053=ORIENTED_EDGE('',*,*,#782,.T.);
#1054=ORIENTED_EDGE('',*,*,#770,.T.);
#1055=ORIENTED_EDGE('',*,*,#772,.T.);
#1056=ORIENTED_EDGE('',*,*,#774,.T.);
#1057=ORIENTED_EDGE('',*,*,#784,.T.);
#1058=ORIENTED_EDGE('',*,*,#787,.T.);
#1059=ORIENTED_EDGE('',*,*,#785,.T.);
#1060=ORIENTED_EDGE('',*,*,#777,.T.);
#1061=ORIENTED_EDGE('',*,*,#779,.T.);
#1062=ORIENTED_EDGE('',*,*,#781,.T.);
#1063=ORIENTED_EDGE('',*,*,#796,.T.);
#1064=ORIENTED_EDGE('',*,*,#812,.T.);
#1065=ORIENTED_EDGE('',*,*,#813,.T.);
#1066=ORIENTED_EDGE('',*,*,#814,.T.);
#1067=ORIENTED_EDGE('',*,*,#815,.T.);
#1068=ORIENTED_EDGE('',*,*,#816,.T.);
#1069=ORIENTED_EDGE('',*,*,#817,.T.);
#1070=ORIENTED_EDGE('',*,*,#818,.T.);
#1071=ORIENTED_EDGE('',*,*,#810,.T.);
#1072=ORIENTED_EDGE('',*,*,#809,.T.);
#1073=ORIENTED_EDGE('',*,*,#806,.T.);
#1074=ORIENTED_EDGE('',*,*,#819,.T.);
#1075=ORIENTED_EDGE('',*,*,#820,.T.);
#1076=ORIENTED_EDGE('',*,*,#821,.T.);
#1077=ORIENTED_EDGE('',*,*,#822,.T.);
#1078=ORIENTED_EDGE('',*,*,#804,.T.);
#1079=ORIENTED_EDGE('',*,*,#801,.T.);
#1080=ORIENTED_EDGE('',*,*,#823,.T.);
#1081=ORIENTED_EDGE('',*,*,#793,.T.);
#1082=ORIENTED_EDGE('',*,*,#792,.T.);
#1083=ORIENTED_EDGE('',*,*,#789,.T.);
#1084=ORIENTED_EDGE('',*,*,#799,.T.);
#1085=ORIENTED_EDGE('',*,*,#797,.T.);
#1086=ORIENTED_EDGE('',*,*,#727,.T.);
#1087=ORIENTED_EDGE('',*,*,#729,.T.);
#1088=ORIENTED_EDGE('',*,*,#824,.T.);
#1089=ORIENTED_EDGE('',*,*,#825,.F.);
#1090=ORIENTED_EDGE('',*,*,#820,.F.);
#1091=ORIENTED_EDGE('',*,*,#826,.F.);
#1092=ORIENTED_EDGE('',*,*,#744,.F.);
#1093=ORIENTED_EDGE('',*,*,#805,.T.);
#1094=ORIENTED_EDGE('',*,*,#745,.T.);
#1095=ORIENTED_EDGE('',*,*,#826,.T.);
#1096=ORIENTED_EDGE('',*,*,#819,.F.);
#1097=ORIENTED_EDGE('',*,*,#803,.T.);
#1098=ORIENTED_EDGE('',*,*,#822,.F.);
#1099=ORIENTED_EDGE('',*,*,#827,.F.);
#1100=ORIENTED_EDGE('',*,*,#742,.F.);
#1101=ORIENTED_EDGE('',*,*,#825,.T.);
#1102=ORIENTED_EDGE('',*,*,#743,.T.);
#1103=ORIENTED_EDGE('',*,*,#827,.T.);
#1104=ORIENTED_EDGE('',*,*,#821,.F.);
#1105=ORIENTED_EDGE('',*,*,#828,.F.);
#1106=ORIENTED_EDGE('',*,*,#751,.T.);
#1107=ORIENTED_EDGE('',*,*,#829,.T.);
#1108=ORIENTED_EDGE('',*,*,#816,.F.);
#1109=ORIENTED_EDGE('',*,*,#830,.F.);
#1110=ORIENTED_EDGE('',*,*,#817,.F.);
#1111=ORIENTED_EDGE('',*,*,#829,.F.);
#1112=ORIENTED_EDGE('',*,*,#750,.F.);
#1113=ORIENTED_EDGE('',*,*,#830,.T.);
#1114=ORIENTED_EDGE('',*,*,#749,.T.);
#1115=ORIENTED_EDGE('',*,*,#811,.T.);
#1116=ORIENTED_EDGE('',*,*,#818,.F.);
#1117=ORIENTED_EDGE('',*,*,#831,.F.);
#1118=ORIENTED_EDGE('',*,*,#813,.F.);
#1119=ORIENTED_EDGE('',*,*,#832,.F.);
#1120=ORIENTED_EDGE('',*,*,#754,.F.);
#1121=ORIENTED_EDGE('',*,*,#795,.T.);
#1122=ORIENTED_EDGE('',*,*,#755,.T.);
#1123=ORIENTED_EDGE('',*,*,#832,.T.);
#1124=ORIENTED_EDGE('',*,*,#812,.F.);
#1125=ORIENTED_EDGE('',*,*,#828,.T.);
#1126=ORIENTED_EDGE('',*,*,#815,.F.);
#1127=ORIENTED_EDGE('',*,*,#833,.F.);
#1128=ORIENTED_EDGE('',*,*,#752,.F.);
#1129=ORIENTED_EDGE('',*,*,#831,.T.);
#1130=ORIENTED_EDGE('',*,*,#753,.T.);
#1131=ORIENTED_EDGE('',*,*,#833,.T.);
#1132=ORIENTED_EDGE('',*,*,#814,.F.);
#1133=ORIENTED_EDGE('',*,*,#800,.T.);
#1134=ORIENTED_EDGE('',*,*,#739,.T.);
#1135=ORIENTED_EDGE('',*,*,#794,.T.);
#1136=ORIENTED_EDGE('',*,*,#823,.F.);
#1137=ORIENTED_EDGE('',*,*,#824,.F.);
#1138=ORIENTED_EDGE('',*,*,#834,.T.);
#1139=ORIENTED_EDGE('',*,*,#767,.F.);
#1140=ORIENTED_EDGE('',*,*,#834,.F.);
#1141=ORIENTED_EDGE('',*,*,#835,.F.);
#1142=ORIENTED_EDGE('',*,*,#836,.T.);
#1143=ORIENTED_EDGE('',*,*,#837,.F.);
#1144=ORIENTED_EDGE('',*,*,#836,.F.);
#1145=ORIENTED_EDGE('',*,*,#838,.F.);
#1146=ORIENTED_EDGE('',*,*,#839,.T.);
#1147=ORIENTED_EDGE('',*,*,#840,.F.);
#1148=ORIENTED_EDGE('',*,*,#841,.F.);
#1149=ORIENTED_EDGE('',*,*,#842,.F.);
#1150=ORIENTED_EDGE('',*,*,#841,.T.);
#1151=ORIENTED_EDGE('',*,*,#843,.F.);
#1152=ORIENTED_EDGE('',*,*,#844,.F.);
#1153=ORIENTED_EDGE('',*,*,#845,.T.);
#1154=ORIENTED_EDGE('',*,*,#844,.T.);
#1155=ORIENTED_EDGE('',*,*,#846,.F.);
#1156=ORIENTED_EDGE('',*,*,#847,.F.);
#1157=ORIENTED_EDGE('',*,*,#848,.T.);
#1158=ORIENTED_EDGE('',*,*,#847,.T.);
#1159=ORIENTED_EDGE('',*,*,#849,.F.);
#1160=ORIENTED_EDGE('',*,*,#850,.F.);
#1161=ORIENTED_EDGE('',*,*,#851,.F.);
#1162=ORIENTED_EDGE('',*,*,#850,.T.);
#1163=ORIENTED_EDGE('',*,*,#852,.F.);
#1164=ORIENTED_EDGE('',*,*,#839,.F.);
#1165=ORIENTED_EDGE('',*,*,#851,.T.);
#1166=ORIENTED_EDGE('',*,*,#838,.T.);
#1167=ORIENTED_EDGE('',*,*,#842,.T.);
#1168=ORIENTED_EDGE('',*,*,#845,.F.);
#1169=ORIENTED_EDGE('',*,*,#848,.F.);
#1170=ORIENTED_EDGE('',*,*,#835,.T.);
#1171=ORIENTED_EDGE('',*,*,#852,.T.);
#1172=ORIENTED_EDGE('',*,*,#849,.T.);
#1173=ORIENTED_EDGE('',*,*,#846,.T.);
#1174=ORIENTED_EDGE('',*,*,#843,.T.);
#1175=ORIENTED_EDGE('',*,*,#840,.T.);
#1176=ORIENTED_EDGE('',*,*,#837,.T.);
#1177=ORIENTED_EDGE('',*,*,#853,.T.);
#1178=ORIENTED_EDGE('',*,*,#854,.T.);
#1179=ORIENTED_EDGE('',*,*,#855,.T.);
#1180=ORIENTED_EDGE('',*,*,#856,.T.);
#1181=ORIENTED_EDGE('',*,*,#857,.T.);
#1182=ORIENTED_EDGE('',*,*,#858,.T.);
#1183=ORIENTED_EDGE('',*,*,#859,.T.);
#1184=ORIENTED_EDGE('',*,*,#860,.F.);
#1185=ORIENTED_EDGE('',*,*,#859,.F.);
#1186=ORIENTED_EDGE('',*,*,#861,.F.);
#1187=ORIENTED_EDGE('',*,*,#862,.T.);
#1188=ORIENTED_EDGE('',*,*,#863,.T.);
#1189=ORIENTED_EDGE('',*,*,#864,.T.);
#1190=ORIENTED_EDGE('',*,*,#865,.T.);
#1191=ORIENTED_EDGE('',*,*,#866,.F.);
#1192=ORIENTED_EDGE('',*,*,#867,.T.);
#1193=ORIENTED_EDGE('',*,*,#862,.F.);
#1194=ORIENTED_EDGE('',*,*,#868,.T.);
#1195=ORIENTED_EDGE('',*,*,#858,.F.);
#1196=ORIENTED_EDGE('',*,*,#869,.F.);
#1197=ORIENTED_EDGE('',*,*,#853,.F.);
#1198=ORIENTED_EDGE('',*,*,#867,.F.);
#1199=ORIENTED_EDGE('',*,*,#870,.T.);
#1200=ORIENTED_EDGE('',*,*,#871,.T.);
#1201=ORIENTED_EDGE('',*,*,#872,.F.);
#1202=ORIENTED_EDGE('',*,*,#864,.F.);
#1203=ORIENTED_EDGE('',*,*,#873,.T.);
#1204=ORIENTED_EDGE('',*,*,#874,.T.);
#1205=ORIENTED_EDGE('',*,*,#875,.F.);
#1206=ORIENTED_EDGE('',*,*,#874,.F.);
#1207=ORIENTED_EDGE('',*,*,#871,.F.);
#1208=ORIENTED_EDGE('',*,*,#854,.F.);
#1209=ORIENTED_EDGE('',*,*,#869,.T.);
#1210=ORIENTED_EDGE('',*,*,#857,.F.);
#1211=ORIENTED_EDGE('',*,*,#855,.F.);
#1212=ORIENTED_EDGE('',*,*,#868,.F.);
#1213=ORIENTED_EDGE('',*,*,#861,.T.);
#1214=ORIENTED_EDGE('',*,*,#856,.F.);
#1215=ORIENTED_EDGE('',*,*,#860,.T.);
#1216=ORIENTED_EDGE('',*,*,#865,.F.);
#1217=ORIENTED_EDGE('',*,*,#872,.T.);
#1218=ORIENTED_EDGE('',*,*,#870,.F.);
#1219=ORIENTED_EDGE('',*,*,#876,.F.);
#1220=ORIENTED_EDGE('',*,*,#863,.F.);
#1221=ORIENTED_EDGE('',*,*,#873,.F.);
#1222=ORIENTED_EDGE('',*,*,#875,.T.);
#1223=ORIENTED_EDGE('',*,*,#876,.T.);
#1224=ORIENTED_EDGE('',*,*,#866,.T.);
#1225=ORIENTED_EDGE('',*,*,#877,.F.);
#1226=ORIENTED_EDGE('',*,*,#878,.T.);
#1227=ORIENTED_EDGE('',*,*,#879,.T.);
#1228=ORIENTED_EDGE('',*,*,#878,.F.);
#1229=ORIENTED_EDGE('',*,*,#880,.F.);
#1230=ORIENTED_EDGE('',*,*,#881,.T.);
#1231=ORIENTED_EDGE('',*,*,#882,.T.);
#1232=ORIENTED_EDGE('',*,*,#881,.F.);
#1233=ORIENTED_EDGE('',*,*,#880,.T.);
#1234=ORIENTED_EDGE('',*,*,#877,.T.);
#1235=ORIENTED_EDGE('',*,*,#882,.F.);
#1236=ORIENTED_EDGE('',*,*,#879,.F.);
#1237=ORIENTED_EDGE('',*,*,#883,.F.);
#1238=ORIENTED_EDGE('',*,*,#884,.T.);
#1239=ORIENTED_EDGE('',*,*,#885,.T.);
#1240=ORIENTED_EDGE('',*,*,#884,.F.);
#1241=ORIENTED_EDGE('',*,*,#883,.T.);
#1242=ORIENTED_EDGE('',*,*,#885,.F.);
#1243=ORIENTED_EDGE('',*,*,#886,.T.);
#1244=ORIENTED_EDGE('',*,*,#887,.T.);
#1245=ORIENTED_EDGE('',*,*,#888,.T.);
#1246=ORIENTED_EDGE('',*,*,#889,.T.);
#1247=ORIENTED_EDGE('',*,*,#887,.F.);
#1248=ORIENTED_EDGE('',*,*,#890,.T.);
#1249=ORIENTED_EDGE('',*,*,#891,.F.);
#1250=ORIENTED_EDGE('',*,*,#892,.T.);
#1251=ORIENTED_EDGE('',*,*,#886,.F.);
#1252=ORIENTED_EDGE('',*,*,#893,.F.);
#1253=ORIENTED_EDGE('',*,*,#894,.F.);
#1254=ORIENTED_EDGE('',*,*,#895,.T.);
#1255=ORIENTED_EDGE('',*,*,#896,.F.);
#1256=ORIENTED_EDGE('',*,*,#890,.F.);
#1257=ORIENTED_EDGE('',*,*,#897,.T.);
#1258=ORIENTED_EDGE('',*,*,#891,.T.);
#1259=ORIENTED_EDGE('',*,*,#896,.T.);
#1260=ORIENTED_EDGE('',*,*,#898,.T.);
#1261=ORIENTED_EDGE('',*,*,#888,.F.);
#1262=ORIENTED_EDGE('',*,*,#892,.F.);
#1263=ORIENTED_EDGE('',*,*,#897,.F.);
#1264=ORIENTED_EDGE('',*,*,#899,.F.);
#1265=ORIENTED_EDGE('',*,*,#900,.F.);
#1266=ORIENTED_EDGE('',*,*,#901,.T.);
#1267=ORIENTED_EDGE('',*,*,#898,.F.);
#1268=ORIENTED_EDGE('',*,*,#895,.F.);
#1269=ORIENTED_EDGE('',*,*,#902,.F.);
#1270=ORIENTED_EDGE('',*,*,#899,.T.);
#1271=ORIENTED_EDGE('',*,*,#889,.F.);
#1272=ORIENTED_EDGE('',*,*,#901,.F.);
#1273=ORIENTED_EDGE('',*,*,#903,.F.);
#1274=ORIENTED_EDGE('',*,*,#893,.T.);
#1275=ORIENTED_EDGE('',*,*,#900,.T.);
#1276=ORIENTED_EDGE('',*,*,#902,.T.);
#1277=ORIENTED_EDGE('',*,*,#894,.T.);
#1278=ORIENTED_EDGE('',*,*,#903,.T.);
#1279=ORIENTED_EDGE('',*,*,#904,.F.);
#1280=ORIENTED_EDGE('',*,*,#905,.T.);
#1281=ORIENTED_EDGE('',*,*,#906,.F.);
#1282=ORIENTED_EDGE('',*,*,#907,.F.);
#1283=ORIENTED_EDGE('',*,*,#908,.F.);
#1284=ORIENTED_EDGE('',*,*,#907,.T.);
#1285=ORIENTED_EDGE('',*,*,#909,.F.);
#1286=ORIENTED_EDGE('',*,*,#910,.F.);
#1287=ORIENTED_EDGE('',*,*,#911,.F.);
#1288=ORIENTED_EDGE('',*,*,#910,.T.);
#1289=ORIENTED_EDGE('',*,*,#912,.F.);
#1290=ORIENTED_EDGE('',*,*,#913,.F.);
#1291=ORIENTED_EDGE('',*,*,#914,.F.);
#1292=ORIENTED_EDGE('',*,*,#913,.T.);
#1293=ORIENTED_EDGE('',*,*,#915,.F.);
#1294=ORIENTED_EDGE('',*,*,#905,.F.);
#1295=ORIENTED_EDGE('',*,*,#915,.T.);
#1296=ORIENTED_EDGE('',*,*,#912,.T.);
#1297=ORIENTED_EDGE('',*,*,#909,.T.);
#1298=ORIENTED_EDGE('',*,*,#906,.T.);
#1299=ORIENTED_EDGE('',*,*,#914,.T.);
#1300=ORIENTED_EDGE('',*,*,#904,.T.);
#1301=ORIENTED_EDGE('',*,*,#908,.T.);
#1302=ORIENTED_EDGE('',*,*,#911,.T.);
#1303=ORIENTED_EDGE('',*,*,#916,.F.);
#1304=ORIENTED_EDGE('',*,*,#917,.T.);
#1305=ORIENTED_EDGE('',*,*,#918,.T.);
#1306=ORIENTED_EDGE('',*,*,#917,.F.);
#1307=ORIENTED_EDGE('',*,*,#916,.T.);
#1308=ORIENTED_EDGE('',*,*,#918,.F.);
#1309=PLANE('',#1542);
#1310=PLANE('',#1546);
#1311=PLANE('',#1547);
#1312=PLANE('',#1566);
#1313=PLANE('',#1569);
#1314=PLANE('',#1570);
#1315=PLANE('',#1573);
#1316=PLANE('',#1580);
#1317=PLANE('',#1583);
#1318=PLANE('',#1590);
#1319=PLANE('',#1593);
#1320=PLANE('',#1596);
#1321=PLANE('',#1599);
#1322=PLANE('',#1607);
#1323=PLANE('',#1609);
#1324=PLANE('',#1610);
#1325=PLANE('',#1612);
#1326=PLANE('',#1614);
#1327=PLANE('',#1616);
#1328=PLANE('',#1617);
#1329=PLANE('',#1629);
#1330=PLANE('',#1630);
#1331=PLANE('',#1631);
#1332=PLANE('',#1638);
#1333=PLANE('',#1639);
#1334=PLANE('',#1642);
#1335=PLANE('',#1643);
#1336=PLANE('',#1644);
#1337=PLANE('',#1645);
#1338=PLANE('',#1646);
#1339=PLANE('',#1647);
#1340=PLANE('',#1648);
#1341=PLANE('',#1656);
#1342=PLANE('',#1657);
#1343=PLANE('',#1662);
#1344=PLANE('',#1663);
#1345=PLANE('',#1668);
#1346=PLANE('',#1669);
#1347=PLANE('',#1673);
#1348=PLANE('',#1674);
#1349=PLANE('',#1675);
#1350=PLANE('',#1676);
#1351=PLANE('',#1678);
#1352=PLANE('',#1679);
#1353=PLANE('',#1680);
#1354=PLANE('',#1681);
#1355=PLANE('',#1682);
#1356=PLANE('',#1683);
#1357=PLANE('',#1688);
#1358=PLANE('',#1689);
#1359=ADVANCED_FACE('',(#197),#1309,.T.);
#1360=ADVANCED_FACE('',(#198),#169,.T.);
#1361=ADVANCED_FACE('',(#199),#1310,.T.);
#1362=ADVANCED_FACE('',(#200,#100),#1311,.T.);
#1363=ADVANCED_FACE('',(#201),#1312,.T.);
#1364=ADVANCED_FACE('',(#202),#170,.T.);
#1365=ADVANCED_FACE('',(#203),#1313,.T.);
#1366=ADVANCED_FACE('',(#204),#1314,.T.);
#1367=ADVANCED_FACE('',(#205),#171,.T.);
#1368=ADVANCED_FACE('',(#206),#1315,.T.);
#1369=ADVANCED_FACE('',(#207),#172,.T.);
#1370=ADVANCED_FACE('',(#208),#173,.T.);
#1371=ADVANCED_FACE('',(#209),#174,.T.);
#1372=ADVANCED_FACE('',(#210),#1316,.T.);
#1373=ADVANCED_FACE('',(#211),#175,.T.);
#1374=ADVANCED_FACE('',(#212),#1317,.T.);
#1375=ADVANCED_FACE('',(#213),#176,.T.);
#1376=ADVANCED_FACE('',(#214),#177,.T.);
#1377=ADVANCED_FACE('',(#215),#178,.T.);
#1378=ADVANCED_FACE('',(#216),#1318,.T.);
#1379=ADVANCED_FACE('',(#217),#179,.T.);
#1380=ADVANCED_FACE('',(#218),#1319,.T.);
#1381=ADVANCED_FACE('',(#219),#180,.T.);
#1382=ADVANCED_FACE('',(#220),#1320,.T.);
#1383=ADVANCED_FACE('',(#221),#181,.T.);
#1384=ADVANCED_FACE('',(#222,#101),#1321,.F.);
#1385=ADVANCED_FACE('',(#223),#182,.T.);
#1386=ADVANCED_FACE('',(#224),#1322,.T.);
#1387=ADVANCED_FACE('',(#225),#183,.T.);
#1388=ADVANCED_FACE('',(#226),#1323,.T.);
#1389=ADVANCED_FACE('',(#227),#1324,.T.);
#1390=ADVANCED_FACE('',(#228),#184,.T.);
#1391=ADVANCED_FACE('',(#229),#1325,.T.);
#1392=ADVANCED_FACE('',(#230),#185,.T.);
#1393=ADVANCED_FACE('',(#231),#1326,.T.);
#1394=ADVANCED_FACE('',(#232),#186,.T.);
#1395=ADVANCED_FACE('',(#233),#1327,.T.);
#1396=ADVANCED_FACE('',(#234),#1328,.T.);
#1397=ADVANCED_FACE('',(#235),#187,.F.);
#1398=ADVANCED_FACE('',(#236),#188,.F.);
#1399=ADVANCED_FACE('',(#237),#66,.T.);
#1400=ADVANCED_FACE('',(#238),#189,.T.);
#1401=ADVANCED_FACE('',(#239),#67,.T.);
#1402=ADVANCED_FACE('',(#240),#190,.F.);
#1403=ADVANCED_FACE('',(#241),#1329,.T.);
#1404=ADVANCED_FACE('',(#242,#102),#1330,.T.);
#1405=ADVANCED_FACE('',(#243,#103),#1331,.F.);
#1406=ADVANCED_FACE('',(#244),#58,.T.);
#1407=ADVANCED_FACE('',(#245),#59,.T.);
#1408=ADVANCED_FACE('',(#246),#1332,.F.);
#1409=ADVANCED_FACE('',(#247),#1333,.F.);
#1410=ADVANCED_FACE('',(#248),#60,.T.);
#1411=ADVANCED_FACE('',(#249),#61,.T.);
#1412=ADVANCED_FACE('',(#250),#1334,.F.);
#1413=ADVANCED_FACE('',(#251),#1335,.F.);
#1414=ADVANCED_FACE('',(#252),#1336,.T.);
#1415=ADVANCED_FACE('',(#253),#1337,.F.);
#1416=ADVANCED_FACE('',(#254),#1338,.F.);
#1417=ADVANCED_FACE('',(#255),#1339,.T.);
#1418=ADVANCED_FACE('',(#256),#1340,.T.);
#1419=ADVANCED_FACE('',(#257),#191,.F.);
#1420=ADVANCED_FACE('',(#258),#192,.T.);
#1421=ADVANCED_FACE('',(#259,#104),#1341,.T.);
#1422=ADVANCED_FACE('',(#260,#105),#1342,.F.);
#1423=ADVANCED_FACE('',(#261),#193,.T.);
#1424=ADVANCED_FACE('',(#262),#1343,.T.);
#1425=ADVANCED_FACE('',(#263),#1344,.F.);
#1426=ADVANCED_FACE('',(#264),#194,.T.);
#1427=ADVANCED_FACE('',(#265),#1345,.T.);
#1428=ADVANCED_FACE('',(#266),#1346,.T.);
#1429=ADVANCED_FACE('',(#267),#195,.T.);
#1430=ADVANCED_FACE('',(#268),#1347,.T.);
#1431=ADVANCED_FACE('',(#269),#1348,.T.);
#1432=ADVANCED_FACE('',(#270),#1349,.T.);
#1433=ADVANCED_FACE('',(#271),#1350,.F.);
#1434=ADVANCED_FACE('',(#272),#1351,.T.);
#1435=ADVANCED_FACE('',(#273),#1352,.T.);
#1436=ADVANCED_FACE('',(#274),#1353,.T.);
#1437=ADVANCED_FACE('',(#275),#1354,.T.);
#1438=ADVANCED_FACE('',(#276),#1355,.T.);
#1439=ADVANCED_FACE('',(#277),#1356,.F.);
#1440=ADVANCED_FACE('',(#278),#196,.T.);
#1441=ADVANCED_FACE('',(#279),#1357,.T.);
#1442=ADVANCED_FACE('',(#280),#1358,.F.);
#1443=CLOSED_SHELL('',(#1359,#1360,#1361,#1362,#1363,#1364,#1365,#1366,
#1367,#1368,#1369,#1370,#1371,#1372,#1373,#1374,#1375,#1376,#1377,#1378,
#1379,#1380,#1381,#1382,#1383,#1384,#1385,#1386,#1387,#1388,#1389,#1390,
#1391,#1392,#1393,#1394,#1395,#1396,#1397));
#1444=CLOSED_SHELL('',(#1398,#1399,#1400,#1401,#1402,#1403,#1404,#1405));
#1445=CLOSED_SHELL('',(#1406,#1407,#1408,#1409,#1410,#1411,#1412,#1413,
#1414,#1415,#1416,#1417,#1418));
#1446=CLOSED_SHELL('',(#1419,#1420,#1421,#1422));
#1447=CLOSED_SHELL('',(#1423,#1424,#1425));
#1448=CLOSED_SHELL('',(#1426,#1427,#1428,#1429,#1430,#1431,#1432,#1433));
#1449=CLOSED_SHELL('',(#1434,#1435,#1436,#1437,#1438,#1439));
#1450=CLOSED_SHELL('',(#1440,#1441,#1442));
#1451=DERIVED_UNIT_ELEMENT(#1467,1.);
#1452=DERIVED_UNIT_ELEMENT(#4081,-3.);
#1453=DERIVED_UNIT_ELEMENT(#1467,1.);
#1454=DERIVED_UNIT_ELEMENT(#4081,-3.);
#1455=DERIVED_UNIT_ELEMENT(#1467,1.);
#1456=DERIVED_UNIT_ELEMENT(#4081,-3.);
#1457=DERIVED_UNIT_ELEMENT(#1467,1.);
#1458=DERIVED_UNIT_ELEMENT(#4081,-3.);
#1459=DERIVED_UNIT_ELEMENT(#1467,1.);
#1460=DERIVED_UNIT_ELEMENT(#4081,-3.);
#1461=DERIVED_UNIT_ELEMENT(#1467,1.);
#1462=DERIVED_UNIT_ELEMENT(#4081,-3.);
#1463=DERIVED_UNIT_ELEMENT(#1467,1.);
#1464=DERIVED_UNIT_ELEMENT(#4081,-3.);
#1465=DERIVED_UNIT_ELEMENT(#1467,1.);
#1466=DERIVED_UNIT_ELEMENT(#4081,-3.);
#1467=(
MASS_UNIT()
NAMED_UNIT(*)
SI_UNIT(.KILO.,.GRAM.)
);
#1468=DERIVED_UNIT((#1451,#1452));
#1469=DERIVED_UNIT((#1453,#1454));
#1470=DERIVED_UNIT((#1455,#1456));
#1471=DERIVED_UNIT((#1457,#1458));
#1472=DERIVED_UNIT((#1459,#1460));
#1473=DERIVED_UNIT((#1461,#1462));
#1474=DERIVED_UNIT((#1463,#1464));
#1475=DERIVED_UNIT((#1465,#1466));
#1476=MEASURE_REPRESENTATION_ITEM('density measure',
POSITIVE_RATIO_MEASURE(7850.),#1468);
#1477=MEASURE_REPRESENTATION_ITEM('density measure',
POSITIVE_RATIO_MEASURE(7850.),#1469);
#1478=MEASURE_REPRESENTATION_ITEM('density measure',
POSITIVE_RATIO_MEASURE(7850.),#1470);
#1479=MEASURE_REPRESENTATION_ITEM('density measure',
POSITIVE_RATIO_MEASURE(7850.),#1471);
#1480=MEASURE_REPRESENTATION_ITEM('density measure',
POSITIVE_RATIO_MEASURE(7850.),#1472);
#1481=MEASURE_REPRESENTATION_ITEM('density measure',
POSITIVE_RATIO_MEASURE(7850.),#1473);
#1482=MEASURE_REPRESENTATION_ITEM('density measure',
POSITIVE_RATIO_MEASURE(7850.),#1474);
#1483=MEASURE_REPRESENTATION_ITEM('density measure',
POSITIVE_RATIO_MEASURE(7850.),#1475);
#1484=PROPERTY_DEFINITION_REPRESENTATION(#1524,#1500);
#1485=PROPERTY_DEFINITION_REPRESENTATION(#1525,#1501);
#1486=PROPERTY_DEFINITION_REPRESENTATION(#1526,#1502);
#1487=PROPERTY_DEFINITION_REPRESENTATION(#1527,#1503);
#1488=PROPERTY_DEFINITION_REPRESENTATION(#1528,#1504);
#1489=PROPERTY_DEFINITION_REPRESENTATION(#1529,#1505);
#1490=PROPERTY_DEFINITION_REPRESENTATION(#1530,#1506);
#1491=PROPERTY_DEFINITION_REPRESENTATION(#1531,#1507);
#1492=PROPERTY_DEFINITION_REPRESENTATION(#1532,#1508);
#1493=PROPERTY_DEFINITION_REPRESENTATION(#1533,#1509);
#1494=PROPERTY_DEFINITION_REPRESENTATION(#1534,#1510);
#1495=PROPERTY_DEFINITION_REPRESENTATION(#1535,#1511);
#1496=PROPERTY_DEFINITION_REPRESENTATION(#1536,#1512);
#1497=PROPERTY_DEFINITION_REPRESENTATION(#1537,#1513);
#1498=PROPERTY_DEFINITION_REPRESENTATION(#1538,#1514);
#1499=PROPERTY_DEFINITION_REPRESENTATION(#1539,#1515);
#1500=REPRESENTATION('material name',(#1516),#4071);
#1501=REPRESENTATION('density',(#1476),#4071);
#1502=REPRESENTATION('material name',(#1517),#4072);
#1503=REPRESENTATION('density',(#1477),#4072);
#1504=REPRESENTATION('material name',(#1518),#4073);
#1505=REPRESENTATION('density',(#1478),#4073);
#1506=REPRESENTATION('material name',(#1519),#4074);
#1507=REPRESENTATION('density',(#1479),#4074);
#1508=REPRESENTATION('material name',(#1520),#4075);
#1509=REPRESENTATION('density',(#1480),#4075);
#1510=REPRESENTATION('material name',(#1521),#4076);
#1511=REPRESENTATION('density',(#1481),#4076);
#1512=REPRESENTATION('material name',(#1522),#4077);
#1513=REPRESENTATION('density',(#1482),#4077);
#1514=REPRESENTATION('material name',(#1523),#4078);
#1515=REPRESENTATION('density',(#1483),#4078);
#1516=DESCRIPTIVE_REPRESENTATION_ITEM('Steel','Steel');
#1517=DESCRIPTIVE_REPRESENTATION_ITEM('Steel','Steel');
#1518=DESCRIPTIVE_REPRESENTATION_ITEM('Steel','Steel');
#1519=DESCRIPTIVE_REPRESENTATION_ITEM('Steel','Steel');
#1520=DESCRIPTIVE_REPRESENTATION_ITEM('Steel','Steel');
#1521=DESCRIPTIVE_REPRESENTATION_ITEM('Steel','Steel');
#1522=DESCRIPTIVE_REPRESENTATION_ITEM('Steel','Steel');
#1523=DESCRIPTIVE_REPRESENTATION_ITEM('Steel','Steel');
#1524=PROPERTY_DEFINITION('material property','material name',#4121);
#1525=PROPERTY_DEFINITION('material property','density of part',#4121);
#1526=PROPERTY_DEFINITION('material property','material name',#4122);
#1527=PROPERTY_DEFINITION('material property','density of part',#4122);
#1528=PROPERTY_DEFINITION('material property','material name',#4123);
#1529=PROPERTY_DEFINITION('material property','density of part',#4123);
#1530=PROPERTY_DEFINITION('material property','material name',#4124);
#1531=PROPERTY_DEFINITION('material property','density of part',#4124);
#1532=PROPERTY_DEFINITION('material property','material name',#4125);
#1533=PROPERTY_DEFINITION('material property','density of part',#4125);
#1534=PROPERTY_DEFINITION('material property','material name',#4126);
#1535=PROPERTY_DEFINITION('material property','density of part',#4126);
#1536=PROPERTY_DEFINITION('material property','material name',#4127);
#1537=PROPERTY_DEFINITION('material property','density of part',#4127);
#1538=PROPERTY_DEFINITION('material property','material name',#4128);
#1539=PROPERTY_DEFINITION('material property','density of part',#4128);
#1540=AXIS2_PLACEMENT_3D('',#2127,#1698,#1699);
#1541=AXIS2_PLACEMENT_3D('',#2128,#1700,#1701);
#1542=AXIS2_PLACEMENT_3D('',#2129,#1702,#1703);
#1543=AXIS2_PLACEMENT_3D('',#2138,#1708,#1709);
#1544=AXIS2_PLACEMENT_3D('',#2142,#1711,#1712);
#1545=AXIS2_PLACEMENT_3D('',#2143,#1713,#1714);
#1546=AXIS2_PLACEMENT_3D('',#2144,#1715,#1716);
#1547=AXIS2_PLACEMENT_3D('',#2150,#1720,#1721);
#1548=AXIS2_PLACEMENT_3D('',#2152,#1722,#1723);
#1549=AXIS2_PLACEMENT_3D('',#2156,#1725,#1726);
#1550=AXIS2_PLACEMENT_3D('',#2160,#1728,#1729);
#1551=AXIS2_PLACEMENT_3D('',#2164,#1731,#1732);
#1552=AXIS2_PLACEMENT_3D('',#2168,#1734,#1735);
#1553=AXIS2_PLACEMENT_3D('',#2172,#1737,#1738);
#1554=AXIS2_PLACEMENT_3D('',#2176,#1740,#1741);
#1555=AXIS2_PLACEMENT_3D('',#2180,#1743,#1744);
#1556=AXIS2_PLACEMENT_3D('',#2184,#1746,#1747);
#1557=AXIS2_PLACEMENT_3D('',#2188,#1749,#1750);
#1558=AXIS2_PLACEMENT_3D('',#2192,#1752,#1753);
#1559=AXIS2_PLACEMENT_3D('',#2196,#1755,#1756);
#1560=AXIS2_PLACEMENT_3D('',#2200,#1758,#1759);
#1561=AXIS2_PLACEMENT_3D('',#2204,#1761,#1762);
#1562=AXIS2_PLACEMENT_3D('',#2208,#1764,#1765);
#1563=AXIS2_PLACEMENT_3D('',#2212,#1767,#1768);
#1564=AXIS2_PLACEMENT_3D('',#2215,#1770,#1771);
#1565=AXIS2_PLACEMENT_3D('',#2217,#1772,#1773);
#1566=AXIS2_PLACEMENT_3D('',#2218,#1774,#1775);
#1567=AXIS2_PLACEMENT_3D('',#2224,#1779,#1780);
#1568=AXIS2_PLACEMENT_3D('',#2227,#1782,#1783);
#1569=AXIS2_PLACEMENT_3D('',#2228,#1784,#1785);
#1570=AXIS2_PLACEMENT_3D('',#2232,#1788,#1789);
#1571=AXIS2_PLACEMENT_3D('',#2238,#1793,#1794);
#1572=AXIS2_PLACEMENT_3D('',#2241,#1796,#1797);
#1573=AXIS2_PLACEMENT_3D('',#2242,#1798,#1799);
#1574=AXIS2_PLACEMENT_3D('',#2246,#1802,#1803);
#1575=AXIS2_PLACEMENT_3D('',#2247,#1804,#1805);
#1576=AXIS2_PLACEMENT_3D('',#2248,#1806,#1807);
#1577=AXIS2_PLACEMENT_3D('',#2251,#1809,#1810);
#1578=AXIS2_PLACEMENT_3D('',#2252,#1811,#1812);
#1579=AXIS2_PLACEMENT_3D('',#2254,#1813,#1814);
#1580=AXIS2_PLACEMENT_3D('',#2256,#1816,#1817);
#1581=AXIS2_PLACEMENT_3D('',#2258,#1819,#1820);
#1582=AXIS2_PLACEMENT_3D('',#2262,#1822,#1823);
#1583=AXIS2_PLACEMENT_3D('',#2264,#1825,#1826);
#1584=AXIS2_PLACEMENT_3D('',#2268,#1829,#1830);
#1585=AXIS2_PLACEMENT_3D('',#2270,#1831,#1832);
#1586=AXIS2_PLACEMENT_3D('',#2272,#1834,#1835);
#1587=AXIS2_PLACEMENT_3D('',#2275,#1837,#1838);
#1588=AXIS2_PLACEMENT_3D('',#2276,#1839,#1840);
#1589=AXIS2_PLACEMENT_3D('',#2278,#1841,#1842);
#1590=AXIS2_PLACEMENT_3D('',#2280,#1844,#1845);
#1591=AXIS2_PLACEMENT_3D('',#2282,#1847,#1848);
#1592=AXIS2_PLACEMENT_3D('',#2286,#1850,#1851);
#1593=AXIS2_PLACEMENT_3D('',#2288,#1853,#1854);
#1594=AXIS2_PLACEMENT_3D('',#2292,#1857,#1858);
#1595=AXIS2_PLACEMENT_3D('',#2296,#1860,#1861);
#1596=AXIS2_PLACEMENT_3D('',#2298,#1863,#1864);
#1597=AXIS2_PLACEMENT_3D('',#2302,#1867,#1868);
#1598=AXIS2_PLACEMENT_3D('',#2304,#1869,#1870);
#1599=AXIS2_PLACEMENT_3D('',#2306,#1872,#1873);
#1600=AXIS2_PLACEMENT_3D('',#2310,#1875,#1876);
#1601=AXIS2_PLACEMENT_3D('',#2314,#1878,#1879);
#1602=AXIS2_PLACEMENT_3D('',#2318,#1881,#1882);
#1603=AXIS2_PLACEMENT_3D('',#2323,#1885,#1886);
#1604=AXIS2_PLACEMENT_3D('',#2326,#1888,#1889);
#1605=AXIS2_PLACEMENT_3D('',#2329,#1891,#1892);
#1606=AXIS2_PLACEMENT_3D('',#2330,#1893,#1894);
#1607=AXIS2_PLACEMENT_3D('',#2333,#1897,#1898);
#1608=AXIS2_PLACEMENT_3D('',#2334,#1899,#1900);
#1609=AXIS2_PLACEMENT_3D('',#2336,#1902,#1903);
#1610=AXIS2_PLACEMENT_3D('',#2337,#1904,#1905);
#1611=AXIS2_PLACEMENT_3D('',#2340,#1908,#1909);
#1612=AXIS2_PLACEMENT_3D('',#2342,#1911,#1912);
#1613=AXIS2_PLACEMENT_3D('',#2343,#1913,#1914);
#1614=AXIS2_PLACEMENT_3D('',#2346,#1917,#1918);
#1615=AXIS2_PLACEMENT_3D('',#2347,#1919,#1920);
#1616=AXIS2_PLACEMENT_3D('',#2349,#1922,#1923);
#1617=AXIS2_PLACEMENT_3D('',#2350,#1924,#1925);
#1618=AXIS2_PLACEMENT_3D('',#2351,#1926,#1927);
#1619=AXIS2_PLACEMENT_3D('',#2353,#1929,#1930);
#1620=AXIS2_PLACEMENT_3D('',#2354,#1931,#1932);
#1621=AXIS2_PLACEMENT_3D('',#2356,#1933,#1934);
#1622=AXIS2_PLACEMENT_3D('',#2359,#1936,#1937);
#1623=AXIS2_PLACEMENT_3D('',#2446,#1940,#1941);
#1624=AXIS2_PLACEMENT_3D('',#2448,#1942,#1943);
#1625=AXIS2_PLACEMENT_3D('',#2450,#1944,#1945);
#1626=AXIS2_PLACEMENT_3D('',#2555,#1948,#1949);
#1627=AXIS2_PLACEMENT_3D('',#2557,#1950,#1951);
#1628=AXIS2_PLACEMENT_3D('',#2559,#1952,#1953);
#1629=AXIS2_PLACEMENT_3D('',#2561,#1955,#1956);
#1630=AXIS2_PLACEMENT_3D('',#2564,#1959,#1960);
#1631=AXIS2_PLACEMENT_3D('',#2565,#1961,#1962);
#1632=AXIS2_PLACEMENT_3D('',#2566,#1963,#1964);
#1633=AXIS2_PLACEMENT_3D('',#2699,#1965,#1966);
#1634=AXIS2_PLACEMENT_3D('',#2700,#1967,#1968);
#1635=AXIS2_PLACEMENT_3D('',#2732,#1969,#1970);
#1636=AXIS2_PLACEMENT_3D('',#3540,#1971,#1972);
#1637=AXIS2_PLACEMENT_3D('',#3541,#1973,#1974);
#1638=AXIS2_PLACEMENT_3D('',#3562,#1975,#1976);
#1639=AXIS2_PLACEMENT_3D('',#3597,#1977,#1978);
#1640=AXIS2_PLACEMENT_3D('',#3898,#1980,#1981);
#1641=AXIS2_PLACEMENT_3D('',#3924,#1982,#1983);
#1642=AXIS2_PLACEMENT_3D('',#3945,#1984,#1985);
#1643=AXIS2_PLACEMENT_3D('',#3946,#1986,#1987);
#1644=AXIS2_PLACEMENT_3D('',#3947,#1988,#1989);
#1645=AXIS2_PLACEMENT_3D('',#3948,#1990,#1991);
#1646=AXIS2_PLACEMENT_3D('',#3950,#1993,#1994);
#1647=AXIS2_PLACEMENT_3D('',#3951,#1995,#1996);
#1648=AXIS2_PLACEMENT_3D('',#3952,#1997,#1998);
#1649=AXIS2_PLACEMENT_3D('',#3953,#1999,#2000);
#1650=AXIS2_PLACEMENT_3D('',#3954,#2001,#2002);
#1651=AXIS2_PLACEMENT_3D('',#3956,#2003,#2004);
#1652=AXIS2_PLACEMENT_3D('',#3959,#2006,#2007);
#1653=AXIS2_PLACEMENT_3D('',#3960,#2008,#2009);
#1654=AXIS2_PLACEMENT_3D('',#3962,#2010,#2011);
#1655=AXIS2_PLACEMENT_3D('',#3965,#2013,#2014);
#1656=AXIS2_PLACEMENT_3D('',#3966,#2015,#2016);
#1657=AXIS2_PLACEMENT_3D('',#3967,#2017,#2018);
#1658=AXIS2_PLACEMENT_3D('',#3968,#2019,#2020);
#1659=AXIS2_PLACEMENT_3D('',#3969,#2021,#2022);
#1660=AXIS2_PLACEMENT_3D('',#3971,#2023,#2024);
#1661=AXIS2_PLACEMENT_3D('',#3974,#2026,#2027);
#1662=AXIS2_PLACEMENT_3D('',#3975,#2028,#2029);
#1663=AXIS2_PLACEMENT_3D('',#3976,#2030,#2031);
#1664=AXIS2_PLACEMENT_3D('',#3977,#2032,#2033);
#1665=AXIS2_PLACEMENT_3D('',#3978,#2034,#2035);
#1666=AXIS2_PLACEMENT_3D('',#3981,#2036,#2037);
#1667=AXIS2_PLACEMENT_3D('',#3985,#2039,#2040);
#1668=AXIS2_PLACEMENT_3D('',#3987,#2042,#2043);
#1669=AXIS2_PLACEMENT_3D('',#3993,#2047,#2048);
#1670=AXIS2_PLACEMENT_3D('',#4000,#2052,#2053);
#1671=AXIS2_PLACEMENT_3D('',#4001,#2054,#2055);
#1672=AXIS2_PLACEMENT_3D('',#4003,#2056,#2057);
#1673=AXIS2_PLACEMENT_3D('',#4005,#2059,#2060);
#1674=AXIS2_PLACEMENT_3D('',#4011,#2064,#2065);
#1675=AXIS2_PLACEMENT_3D('',#4013,#2067,#2068);
#1676=AXIS2_PLACEMENT_3D('',#4015,#2070,#2071);
#1677=AXIS2_PLACEMENT_3D('',#4016,#2072,#2073);
#1678=AXIS2_PLACEMENT_3D('',#4017,#2074,#2075);
#1679=AXIS2_PLACEMENT_3D('',#4026,#2080,#2081);
#1680=AXIS2_PLACEMENT_3D('',#4032,#2085,#2086);
#1681=AXIS2_PLACEMENT_3D('',#4038,#2090,#2091);
#1682=AXIS2_PLACEMENT_3D('',#4041,#2094,#2095);
#1683=AXIS2_PLACEMENT_3D('',#4042,#2096,#2097);
#1684=AXIS2_PLACEMENT_3D('',#4043,#2098,#2099);
#1685=AXIS2_PLACEMENT_3D('',#4044,#2100,#2101);
#1686=AXIS2_PLACEMENT_3D('',#4046,#2102,#2103);
#1687=AXIS2_PLACEMENT_3D('',#4049,#2105,#2106);
#1688=AXIS2_PLACEMENT_3D('',#4050,#2107,#2108);
#1689=AXIS2_PLACEMENT_3D('',#4051,#2109,#2110);
#1690=AXIS2_PLACEMENT_3D('',#4052,#2111,#2112);
#1691=AXIS2_PLACEMENT_3D('',#4053,#2113,#2114);
#1692=AXIS2_PLACEMENT_3D('',#4054,#2115,#2116);
#1693=AXIS2_PLACEMENT_3D('',#4055,#2117,#2118);
#1694=AXIS2_PLACEMENT_3D('',#4056,#2119,#2120);
#1695=AXIS2_PLACEMENT_3D('',#4057,#2121,#2122);
#1696=AXIS2_PLACEMENT_3D('',#4058,#2123,#2124);
#1697=AXIS2_PLACEMENT_3D('',#4059,#2125,#2126);
#1698=DIRECTION('axis',(0.,0.,1.));
#1699=DIRECTION('refdir',(1.,0.,0.));
#1700=DIRECTION('axis',(0.,0.,1.));
#1701=DIRECTION('refdir',(1.,0.,0.));
#1702=DIRECTION('center_axis',(0.500081199337214,0.,0.865978518249416));
#1703=DIRECTION('ref_axis',(-0.865978518249416,0.,0.500081199337214));
#1704=DIRECTION('',(0.,-1.,0.));
#1705=DIRECTION('',(-0.865978518249416,0.,0.500081199337214));
#1706=DIRECTION('',(0.,-1.,0.));
#1707=DIRECTION('',(-0.865978518249416,0.,0.500081199337214));
#1708=DIRECTION('center_axis',(0.,-1.,0.));
#1709=DIRECTION('ref_axis',(-0.985840852699883,0.,-0.167683669890564));
#1710=DIRECTION('',(0.,1.,0.));
#1711=DIRECTION('center_axis',(0.,-1.,0.));
#1712=DIRECTION('ref_axis',(-0.985840852699883,0.,-0.167683669890564));
#1713=DIRECTION('center_axis',(0.,1.,0.));
#1714=DIRECTION('ref_axis',(-0.985840852699883,0.,-0.167683669890564));
#1715=DIRECTION('center_axis',(0.173740515882331,0.,0.984791466829878));
#1716=DIRECTION('ref_axis',(-0.984791466829877,0.,0.173740515882331));
#1717=DIRECTION('',(-0.984791466829877,0.,0.173740515882331));
#1718=DIRECTION('',(0.,-1.,0.));
#1719=DIRECTION('',(-0.984791466829877,0.,0.173740515882331));
#1720=DIRECTION('center_axis',(0.,1.,0.));
#1721=DIRECTION('ref_axis',(1.,0.,0.));
#1722=DIRECTION('center_axis',(0.,1.,0.));
#1723=DIRECTION('ref_axis',(-0.983738567360713,0.,0.179606322514249));
#1724=DIRECTION('',(-0.642715779886306,0.,0.766104709739562));
#1725=DIRECTION('center_axis',(0.,1.,0.));
#1726=DIRECTION('ref_axis',(-0.862982892362843,0.,0.505233141716833));
#1727=DIRECTION('',(-0.341932032994227,0.,0.939724685645979));
#1728=DIRECTION('center_axis',(0.,1.,0.));
#1729=DIRECTION('ref_axis',(-0.638138744274974,0.,0.769921387581329));
#1730=DIRECTION('',(9.37634563086646E-5,0.,0.999999995604207));
#1731=DIRECTION('center_axis',(0.,1.,0.));
#1732=DIRECTION('ref_axis',(-0.336325645702715,0.,0.941745751274011));
#1733=DIRECTION('',(0.342108250650212,0.,0.939660547664449));
#1734=DIRECTION('center_axis',(0.,1.,0.));
#1735=DIRECTION('ref_axis',(0.00605328937917962,0.,0.999981678676011));
#1736=DIRECTION('',(0.642859433835651,0.,0.765984169763649));
#1737=DIRECTION('center_axis',(0.,1.,0.));
#1738=DIRECTION('ref_axis',(0.347702108424909,0.,0.937605057471894));
#1739=DIRECTION('',(0.866072281705725,0.,0.499918796266994));
#1740=DIRECTION('center_axis',(0.,1.,0.));
#1741=DIRECTION('ref_axis',(0.647412921657998,0.,0.762139428759762));
#1742=DIRECTION('',(0.984824030536517,0.,0.173555837924887));
#1743=DIRECTION('center_axis',(0.,1.,0.));
#1744=DIRECTION('ref_axis',(0.869036181742023,0.,0.494748536959177));
#1745=DIRECTION('',(0.984791466829877,0.,-0.173740515882331));
#1746=DIRECTION('center_axis',(0.,1.,0.));
#1747=DIRECTION('ref_axis',(0.985840852699883,0.,0.167683669890565));
#1748=DIRECTION('',(0.865978518249416,0.,-0.500081199337213));
#1749=DIRECTION('center_axis',(0.,1.,0.));
#1750=DIRECTION('ref_axis',(0.983738567360713,0.,-0.179606322514249));
#1751=DIRECTION('',(0.642715779886305,0.,-0.766104709739562));
#1752=DIRECTION('center_axis',(0.,1.,0.));
#1753=DIRECTION('ref_axis',(0.862982892362843,0.,-0.505233141716833));
#1754=DIRECTION('',(0.341932032994227,0.,-0.93972468564598));
#1755=DIRECTION('center_axis',(0.,1.,0.));
#1756=DIRECTION('ref_axis',(0.638138744274974,0.,-0.769921387581329));
#1757=DIRECTION('',(-9.37634563085422E-5,0.,-0.999999995604207));
#1758=DIRECTION('center_axis',(0.,1.,0.));
#1759=DIRECTION('ref_axis',(0.336325645702715,0.,-0.941745751274011));
#1760=DIRECTION('',(-0.342108250650212,0.,-0.939660547664449));
#1761=DIRECTION('center_axis',(0.,1.,0.));
#1762=DIRECTION('ref_axis',(-0.00605328937917962,0.,-0.999981678676011));
#1763=DIRECTION('',(-0.642859433835651,0.,-0.765984169763649));
#1764=DIRECTION('center_axis',(0.,1.,0.));
#1765=DIRECTION('ref_axis',(-0.347702108424908,0.,-0.937605057471894));
#1766=DIRECTION('',(-0.866072281705724,0.,-0.499918796266994));
#1767=DIRECTION('center_axis',(0.,1.,0.));
#1768=DIRECTION('ref_axis',(-0.647412921657998,0.,-0.762139428759761));
#1769=DIRECTION('',(-0.984824030536517,0.,-0.173555837924887));
#1770=DIRECTION('center_axis',(0.,1.,0.));
#1771=DIRECTION('ref_axis',(-0.869036181742022,0.,-0.494748536959177));
#1772=DIRECTION('center_axis',(0.,-1.,0.));
#1773=DIRECTION('ref_axis',(1.,0.,0.));
#1774=DIRECTION('center_axis',(-0.173555837924887,0.,0.984824030536517));
#1775=DIRECTION('ref_axis',(-0.984824030536517,0.,-0.173555837924887));
#1776=DIRECTION('',(0.,-1.,0.));
#1777=DIRECTION('',(0.,-1.,0.));
#1778=DIRECTION('',(-0.984824030536517,0.,-0.173555837924887));
#1779=DIRECTION('center_axis',(0.,-1.,0.));
#1780=DIRECTION('ref_axis',(-0.647412921657998,0.,-0.762139428759761));
#1781=DIRECTION('',(0.,1.,0.));
#1782=DIRECTION('center_axis',(0.,-1.,0.));
#1783=DIRECTION('ref_axis',(-0.647412921657998,0.,-0.762139428759761));
#1784=DIRECTION('center_axis',(-0.499918796266994,0.,0.866072281705724));
#1785=DIRECTION('ref_axis',(-0.866072281705724,0.,-0.499918796266994));
#1786=DIRECTION('',(0.,-1.,0.));
#1787=DIRECTION('',(-0.866072281705724,0.,-0.499918796266994));
#1788=DIRECTION('center_axis',(-0.939660547664449,0.,0.342108250650212));
#1789=DIRECTION('ref_axis',(-0.342108250650212,0.,-0.939660547664449));
#1790=DIRECTION('',(0.,-1.,0.));
#1791=DIRECTION('',(0.,-1.,0.));
#1792=DIRECTION('',(-0.342108250650212,0.,-0.939660547664449));
#1793=DIRECTION('center_axis',(0.,-1.,0.));
#1794=DIRECTION('ref_axis',(0.336325645702715,0.,-0.941745751274011));
#1795=DIRECTION('',(0.,1.,0.));
#1796=DIRECTION('center_axis',(0.,-1.,0.));
#1797=DIRECTION('ref_axis',(0.336325645702715,0.,-0.941745751274011));
#1798=DIRECTION('center_axis',(-0.999999995604207,0.,9.37634563085422E-5));
#1799=DIRECTION('ref_axis',(-9.37634563085422E-5,0.,-0.999999995604207));
#1800=DIRECTION('',(0.,-1.,0.));
#1801=DIRECTION('',(-9.37634563085422E-5,0.,-0.999999995604207));
#1802=DIRECTION('center_axis',(0.,-1.,0.));
#1803=DIRECTION('ref_axis',(-0.869036181742022,0.,-0.494748536959177));
#1804=DIRECTION('center_axis',(0.,-1.,0.));
#1805=DIRECTION('ref_axis',(-0.869036181742022,0.,-0.494748536959177));
#1806=DIRECTION('center_axis',(0.,-1.,0.));
#1807=DIRECTION('ref_axis',(-0.347702108424908,0.,-0.937605057471894));
#1808=DIRECTION('',(0.,1.,0.));
#1809=DIRECTION('center_axis',(0.,-1.,0.));
#1810=DIRECTION('ref_axis',(-0.347702108424908,0.,-0.937605057471894));
#1811=DIRECTION('center_axis',(0.,-1.,0.));
#1812=DIRECTION('ref_axis',(-0.00605328937917962,0.,-0.999981678676011));
#1813=DIRECTION('center_axis',(0.,-1.,0.));
#1814=DIRECTION('ref_axis',(-0.00605328937917962,0.,-0.999981678676011));
#1815=DIRECTION('',(0.,-1.,0.));
#1816=DIRECTION('center_axis',(-0.765984169763649,0.,0.642859433835651));
#1817=DIRECTION('ref_axis',(-0.642859433835651,0.,-0.765984169763649));
#1818=DIRECTION('',(-0.642859433835651,0.,-0.765984169763649));
#1819=DIRECTION('center_axis',(0.,-1.,0.));
#1820=DIRECTION('ref_axis',(-0.862982892362843,0.,0.505233141716833));
#1821=DIRECTION('',(0.,1.,0.));
#1822=DIRECTION('center_axis',(0.,-1.,0.));
#1823=DIRECTION('ref_axis',(-0.862982892362843,0.,0.505233141716833));
#1824=DIRECTION('',(0.,-1.,0.));
#1825=DIRECTION('center_axis',(0.939724685645979,0.,0.341932032994227));
#1826=DIRECTION('ref_axis',(-0.341932032994227,0.,0.939724685645979));
#1827=DIRECTION('',(0.,-1.,0.));
#1828=DIRECTION('',(-0.341932032994227,0.,0.939724685645979));
#1829=DIRECTION('center_axis',(0.,-1.,0.));
#1830=DIRECTION('ref_axis',(-0.638138744274974,0.,0.769921387581329));
#1831=DIRECTION('center_axis',(0.,-1.,0.));
#1832=DIRECTION('ref_axis',(-0.638138744274974,0.,0.769921387581329));
#1833=DIRECTION('',(0.,-1.,0.));
#1834=DIRECTION('center_axis',(0.,-1.,0.));
#1835=DIRECTION('ref_axis',(0.638138744274974,0.,-0.769921387581329));
#1836=DIRECTION('',(0.,1.,0.));
#1837=DIRECTION('center_axis',(0.,-1.,0.));
#1838=DIRECTION('ref_axis',(0.638138744274974,0.,-0.769921387581329));
#1839=DIRECTION('center_axis',(0.,-1.,0.));
#1840=DIRECTION('ref_axis',(-0.983738567360713,0.,0.179606322514249));
#1841=DIRECTION('center_axis',(0.,-1.,0.));
#1842=DIRECTION('ref_axis',(-0.983738567360713,0.,0.179606322514249));
#1843=DIRECTION('',(0.,-1.,0.));
#1844=DIRECTION('center_axis',(0.766104709739562,0.,0.642715779886306));
#1845=DIRECTION('ref_axis',(-0.642715779886306,0.,0.766104709739562));
#1846=DIRECTION('',(-0.642715779886306,0.,0.766104709739562));
#1847=DIRECTION('center_axis',(0.,-1.,0.));
#1848=DIRECTION('ref_axis',(-0.336325645702715,0.,0.941745751274011));
#1849=DIRECTION('',(0.,1.,0.));
#1850=DIRECTION('center_axis',(0.,-1.,0.));
#1851=DIRECTION('ref_axis',(-0.336325645702715,0.,0.941745751274011));
#1852=DIRECTION('',(0.,-1.,0.));
#1853=DIRECTION('center_axis',(0.939660547664449,0.,-0.342108250650212));
#1854=DIRECTION('ref_axis',(0.342108250650212,0.,0.939660547664449));
#1855=DIRECTION('',(0.,-1.,0.));
#1856=DIRECTION('',(0.342108250650212,0.,0.939660547664449));
#1857=DIRECTION('center_axis',(0.,-1.,0.));
#1858=DIRECTION('ref_axis',(0.647412921657998,0.,0.762139428759762));
#1859=DIRECTION('',(0.,1.,0.));
#1860=DIRECTION('center_axis',(0.,-1.,0.));
#1861=DIRECTION('ref_axis',(0.647412921657998,0.,0.762139428759762));
#1862=DIRECTION('',(0.,-1.,0.));
#1863=DIRECTION('center_axis',(0.173555837924887,0.,-0.984824030536517));
#1864=DIRECTION('ref_axis',(0.984824030536517,0.,0.173555837924887));
#1865=DIRECTION('',(0.,-1.,0.));
#1866=DIRECTION('',(0.984824030536517,0.,0.173555837924887));
#1867=DIRECTION('center_axis',(0.,-1.,0.));
#1868=DIRECTION('ref_axis',(0.869036181742023,0.,0.494748536959177));
#1869=DIRECTION('center_axis',(0.,-1.,0.));
#1870=DIRECTION('ref_axis',(0.869036181742023,0.,0.494748536959177));
#1871=DIRECTION('',(0.,-1.,0.));
#1872=DIRECTION('center_axis',(0.,1.,0.));
#1873=DIRECTION('ref_axis',(1.,0.,0.));
#1874=DIRECTION('',(0.341932032994227,0.,-0.93972468564598));
#1875=DIRECTION('center_axis',(0.,-1.,0.));
#1876=DIRECTION('ref_axis',(0.862982892362843,0.,-0.505233141716833));
#1877=DIRECTION('',(0.642715779886305,0.,-0.766104709739562));
#1878=DIRECTION('center_axis',(0.,-1.,0.));
#1879=DIRECTION('ref_axis',(0.983738567360713,0.,-0.179606322514249));
#1880=DIRECTION('',(0.865978518249416,0.,-0.500081199337213));
#1881=DIRECTION('center_axis',(0.,-1.,0.));
#1882=DIRECTION('ref_axis',(0.985840852699883,0.,0.167683669890565));
#1883=DIRECTION('',(0.984791466829877,0.,-0.173740515882331));
#1884=DIRECTION('',(0.866072281705725,0.,0.499918796266994));
#1885=DIRECTION('center_axis',(0.,-1.,0.));
#1886=DIRECTION('ref_axis',(0.347702108424909,0.,0.937605057471894));
#1887=DIRECTION('',(0.642859433835651,0.,0.765984169763649));
#1888=DIRECTION('center_axis',(0.,-1.,0.));
#1889=DIRECTION('ref_axis',(0.00605328937917962,0.,0.999981678676011));
#1890=DIRECTION('',(9.37634563086646E-5,0.,0.999999995604207));
#1891=DIRECTION('center_axis',(0.,1.,0.));
#1892=DIRECTION('ref_axis',(1.,0.,0.));
#1893=DIRECTION('center_axis',(0.,-1.,0.));
#1894=DIRECTION('ref_axis',(0.347702108424909,0.,0.937605057471894));
#1895=DIRECTION('',(0.,1.,0.));
#1896=DIRECTION('',(0.,-1.,0.));
#1897=DIRECTION('center_axis',(0.499918796266994,0.,-0.866072281705725));
#1898=DIRECTION('ref_axis',(0.866072281705725,0.,0.499918796266994));
#1899=DIRECTION('center_axis',(0.,-1.,0.));
#1900=DIRECTION('ref_axis',(0.00605328937917962,0.,0.999981678676011));
#1901=DIRECTION('',(0.,-1.,0.));
#1902=DIRECTION('center_axis',(0.765984169763649,0.,-0.642859433835651));
#1903=DIRECTION('ref_axis',(0.642859433835651,0.,0.765984169763649));
#1904=DIRECTION('center_axis',(-0.500081199337213,0.,-0.865978518249416));
#1905=DIRECTION('ref_axis',(0.865978518249416,0.,-0.500081199337213));
#1906=DIRECTION('',(0.,-1.,0.));
#1907=DIRECTION('',(0.,-1.,0.));
#1908=DIRECTION('center_axis',(0.,-1.,0.));
#1909=DIRECTION('ref_axis',(0.985840852699883,0.,0.167683669890565));
#1910=DIRECTION('',(0.,1.,0.));
#1911=DIRECTION('center_axis',(-0.173740515882331,0.,-0.984791466829877));
#1912=DIRECTION('ref_axis',(0.984791466829877,0.,-0.173740515882331));
#1913=DIRECTION('center_axis',(0.,-1.,0.));
#1914=DIRECTION('ref_axis',(0.862982892362843,0.,-0.505233141716833));
#1915=DIRECTION('',(0.,1.,0.));
#1916=DIRECTION('',(0.,-1.,0.));
#1917=DIRECTION('center_axis',(-0.93972468564598,0.,-0.341932032994227));
#1918=DIRECTION('ref_axis',(0.341932032994227,0.,-0.93972468564598));
#1919=DIRECTION('center_axis',(0.,-1.,0.));
#1920=DIRECTION('ref_axis',(0.983738567360713,0.,-0.179606322514249));
#1921=DIRECTION('',(0.,-1.,0.));
#1922=DIRECTION('center_axis',(-0.766104709739562,0.,-0.642715779886305));
#1923=DIRECTION('ref_axis',(0.642715779886305,0.,-0.766104709739562));
#1924=DIRECTION('center_axis',(0.999999995604207,0.,-9.37634563086646E-5));
#1925=DIRECTION('ref_axis',(9.37634563086646E-5,0.,0.999999995604207));
#1926=DIRECTION('center_axis',(0.,-1.,0.));
#1927=DIRECTION('ref_axis',(1.,0.,0.));
#1928=DIRECTION('',(0.,1.,0.));
#1929=DIRECTION('axis',(0.,0.,1.));
#1930=DIRECTION('refdir',(1.,0.,0.));
#1931=DIRECTION('center_axis',(0.,-1.,0.));
#1932=DIRECTION('ref_axis',(1.,0.,0.));
#1933=DIRECTION('center_axis',(0.,-1.,0.));
#1934=DIRECTION('ref_axis',(1.,0.,0.));
#1935=DIRECTION('',(0.,-1.,0.));
#1936=DIRECTION('center_axis',(0.,1.,0.));
#1937=DIRECTION('ref_axis',(1.,0.,0.));
#1938=DIRECTION('',(0.,-1.,0.));
#1939=DIRECTION('',(0.,-1.,0.));
#1940=DIRECTION('center_axis',(0.,-1.,0.));
#1941=DIRECTION('ref_axis',(1.,0.,0.));
#1942=DIRECTION('center_axis',(0.,1.,0.));
#1943=DIRECTION('ref_axis',(1.,0.,0.));
#1944=DIRECTION('center_axis',(0.,-1.,0.));
#1945=DIRECTION('ref_axis',(1.,0.,0.));
#1946=DIRECTION('',(0.,-1.,0.));
#1947=DIRECTION('',(0.,-1.,0.));
#1948=DIRECTION('center_axis',(0.,-1.,0.));
#1949=DIRECTION('ref_axis',(-0.332459503726204,0.,0.943117531584546));
#1950=DIRECTION('center_axis',(0.,1.,0.));
#1951=DIRECTION('ref_axis',(-0.332459503726204,0.,0.943117531584546));
#1952=DIRECTION('center_axis',(0.,1.,0.));
#1953=DIRECTION('ref_axis',(-0.332459503726204,0.,0.943117531584546));
#1954=DIRECTION('',(0.,-1.,0.));
#1955=DIRECTION('center_axis',(-0.999999995604207,0.,9.37634563086646E-5));
#1956=DIRECTION('ref_axis',(-9.37634563086646E-5,0.,-0.999999995604207));
#1957=DIRECTION('',(9.37634563086646E-5,0.,0.999999995604207));
#1958=DIRECTION('',(-9.37634563086646E-5,0.,-0.999999995604207));
#1959=DIRECTION('center_axis',(0.,1.,0.));
#1960=DIRECTION('ref_axis',(1.,0.,0.));
#1961=DIRECTION('center_axis',(0.,1.,0.));
#1962=DIRECTION('ref_axis',(1.,0.,0.));
#1963=DIRECTION('axis',(0.,0.,1.));
#1964=DIRECTION('refdir',(1.,0.,0.));
#1965=DIRECTION('center_axis',(0.,-0.991319117631768,-0.131477781460493));
#1966=DIRECTION('ref_axis',(1.,0.,0.));
#1967=DIRECTION('center_axis',(0.,-0.991319117631768,-0.131477781460493));
#1968=DIRECTION('ref_axis',(1.,0.,0.));
#1969=DIRECTION('center_axis',(0.,0.072334353589932,-0.997380439597011));
#1970=DIRECTION('ref_axis',(1.,0.,0.));
#1971=DIRECTION('center_axis',(1.22464679914735E-15,1.,0.));
#1972=DIRECTION('ref_axis',(-1.,1.22464679914735E-15,0.));
#1973=DIRECTION('center_axis',(-1.22464679914735E-15,-1.,0.));
#1974=DIRECTION('ref_axis',(-1.,1.22464679914735E-15,0.));
#1975=DIRECTION('center_axis',(0.,1.,0.));
#1976=DIRECTION('ref_axis',(0.,0.,1.));
#1977=DIRECTION('center_axis',(1.22464679914735E-15,1.,0.));
#1978=DIRECTION('ref_axis',(0.,0.,1.));
#1979=DIRECTION('',(1.,-1.22464679914735E-15,9.23361932986486E-15));
#1980=DIRECTION('center_axis',(0.,0.991319117631768,0.13147778146049));
#1981=DIRECTION('ref_axis',(-1.,0.,0.));
#1982=DIRECTION('center_axis',(0.,0.999879786123581,-0.0155052668942604));
#1983=DIRECTION('ref_axis',(-1.,0.,0.));
#1984=DIRECTION('center_axis',(0.,-0.991319117631768,-0.131477781460493));
#1985=DIRECTION('ref_axis',(0.,0.131477781460493,-0.991319117631768));
#1986=DIRECTION('center_axis',(0.,-0.991319117631768,-0.131477781460493));
#1987=DIRECTION('ref_axis',(0.,0.131477781460493,-0.991319117631768));
#1988=DIRECTION('center_axis',(0.,0.072334353589932,-0.997380439597011));
#1989=DIRECTION('ref_axis',(0.,0.997380439597011,0.072334353589932));
#1990=DIRECTION('center_axis',(0.,0.991319117631768,0.13147778146049));
#1991=DIRECTION('ref_axis',(0.,-0.13147778146049,0.991319117631768));
#1992=DIRECTION('',(-1.,1.22464679914735E-15,-9.23361932986486E-15));
#1993=DIRECTION('center_axis',(0.,0.991319117631768,0.13147778146049));
#1994=DIRECTION('ref_axis',(0.,-0.13147778146049,0.991319117631768));
#1995=DIRECTION('center_axis',(0.,0.999879786123581,-0.0155052668942604));
#1996=DIRECTION('ref_axis',(0.,0.0155052668942604,0.999879786123581));
#1997=DIRECTION('center_axis',(1.22464679914735E-15,1.,0.));
#1998=DIRECTION('ref_axis',(0.,0.,1.));
#1999=DIRECTION('axis',(0.,0.,1.));
#2000=DIRECTION('refdir',(1.,0.,0.));
#2001=DIRECTION('center_axis',(0.,-1.,0.));
#2002=DIRECTION('ref_axis',(1.,0.,0.));
#2003=DIRECTION('center_axis',(0.,1.,0.));
#2004=DIRECTION('ref_axis',(1.,0.,0.));
#2005=DIRECTION('',(0.,1.,0.));
#2006=DIRECTION('center_axis',(0.,1.,0.));
#2007=DIRECTION('ref_axis',(1.,0.,0.));
#2008=DIRECTION('center_axis',(0.,-1.,0.));
#2009=DIRECTION('ref_axis',(1.,0.,0.));
#2010=DIRECTION('center_axis',(0.,-1.,0.));
#2011=DIRECTION('ref_axis',(1.,0.,0.));
#2012=DIRECTION('',(0.,1.,0.));
#2013=DIRECTION('center_axis',(0.,-1.,0.));
#2014=DIRECTION('ref_axis',(1.,0.,0.));
#2015=DIRECTION('center_axis',(0.,-1.,0.));
#2016=DIRECTION('ref_axis',(1.,0.,0.));
#2017=DIRECTION('center_axis',(0.,-1.,0.));
#2018=DIRECTION('ref_axis',(1.,0.,0.));
#2019=DIRECTION('axis',(0.,0.,1.));
#2020=DIRECTION('refdir',(1.,0.,0.));
#2021=DIRECTION('center_axis',(0.,-1.,0.));
#2022=DIRECTION('ref_axis',(1.,0.,0.));
#2023=DIRECTION('center_axis',(0.,-1.,0.));
#2024=DIRECTION('ref_axis',(1.,0.,0.));
#2025=DIRECTION('',(0.,1.,0.));
#2026=DIRECTION('center_axis',(0.,-1.,0.));
#2027=DIRECTION('ref_axis',(1.,0.,0.));
#2028=DIRECTION('center_axis',(0.,-1.,0.));
#2029=DIRECTION('ref_axis',(1.,0.,0.));
#2030=DIRECTION('center_axis',(0.,-1.,0.));
#2031=DIRECTION('ref_axis',(1.,0.,0.));
#2032=DIRECTION('axis',(0.,0.,1.));
#2033=DIRECTION('refdir',(1.,0.,0.));
#2034=DIRECTION('center_axis',(0.,0.,1.));
#2035=DIRECTION('ref_axis',(0.707106781186548,-0.707106781186547,0.));
#2036=DIRECTION('center_axis',(0.,0.,-1.));
#2037=DIRECTION('ref_axis',(0.707106781186548,-0.707106781186547,0.));
#2038=DIRECTION('',(0.,0.,-1.));
#2039=DIRECTION('center_axis',(0.,0.,1.));
#2040=DIRECTION('ref_axis',(0.707106781186548,-0.707106781186547,0.));
#2041=DIRECTION('',(0.,0.,1.));
#2042=DIRECTION('center_axis',(0.,-1.,0.));
#2043=DIRECTION('ref_axis',(0.,0.,-1.));
#2044=DIRECTION('',(-1.,0.,0.));
#2045=DIRECTION('',(0.,0.,1.));
#2046=DIRECTION('',(1.,0.,0.));
#2047=DIRECTION('center_axis',(0.,0.,1.));
#2048=DIRECTION('ref_axis',(-1.,0.,0.));
#2049=DIRECTION('',(0.,-1.,0.));
#2050=DIRECTION('',(1.,0.,0.));
#2051=DIRECTION('',(0.,-1.,0.));
#2052=DIRECTION('center_axis',(0.,0.,-1.));
#2053=DIRECTION('ref_axis',(-0.707106781186548,-0.707106781186547,0.));
#2054=DIRECTION('center_axis',(0.,0.,-1.));
#2055=DIRECTION('ref_axis',(-0.707106781186548,-0.707106781186547,0.));
#2056=DIRECTION('center_axis',(0.,0.,1.));
#2057=DIRECTION('ref_axis',(-0.707106781186548,-0.707106781186547,0.));
#2058=DIRECTION('',(0.,0.,-1.));
#2059=DIRECTION('center_axis',(0.,0.,-1.));
#2060=DIRECTION('ref_axis',(1.,0.,0.));
#2061=DIRECTION('',(0.,-1.,0.));
#2062=DIRECTION('',(-1.,0.,0.));
#2063=DIRECTION('',(0.,-1.,0.));
#2064=DIRECTION('center_axis',(-1.,0.,0.));
#2065=DIRECTION('ref_axis',(0.,0.,-1.));
#2066=DIRECTION('',(0.,0.,1.));
#2067=DIRECTION('center_axis',(1.,0.,0.));
#2068=DIRECTION('ref_axis',(0.,0.,1.));
#2069=DIRECTION('',(0.,0.,-1.));
#2070=DIRECTION('center_axis',(0.,-1.,0.));
#2071=DIRECTION('ref_axis',(1.,0.,0.));
#2072=DIRECTION('axis',(0.,0.,1.));
#2073=DIRECTION('refdir',(1.,0.,0.));
#2074=DIRECTION('center_axis',(1.,0.,0.));
#2075=DIRECTION('ref_axis',(0.,0.,-1.));
#2076=DIRECTION('',(0.,0.,1.));
#2077=DIRECTION('',(0.,1.,0.));
#2078=DIRECTION('',(0.,0.,-1.));
#2079=DIRECTION('',(0.,1.,0.));
#2080=DIRECTION('center_axis',(0.,0.,1.));
#2081=DIRECTION('ref_axis',(1.,0.,0.));
#2082=DIRECTION('',(-1.,0.,0.));
#2083=DIRECTION('',(1.,0.,0.));
#2084=DIRECTION('',(0.,1.,0.));
#2085=DIRECTION('center_axis',(-1.,0.,0.));
#2086=DIRECTION('ref_axis',(0.,0.,1.));
#2087=DIRECTION('',(0.,0.,-1.));
#2088=DIRECTION('',(0.,0.,1.));
#2089=DIRECTION('',(0.,1.,0.));
#2090=DIRECTION('center_axis',(0.,0.,-1.));
#2091=DIRECTION('ref_axis',(-1.,0.,0.));
#2092=DIRECTION('',(1.,0.,0.));
#2093=DIRECTION('',(-1.,0.,0.));
#2094=DIRECTION('center_axis',(0.,1.,0.));
#2095=DIRECTION('ref_axis',(0.,0.,1.));
#2096=DIRECTION('center_axis',(0.,1.,0.));
#2097=DIRECTION('ref_axis',(1.,0.,0.));
#2098=DIRECTION('axis',(0.,0.,1.));
#2099=DIRECTION('refdir',(1.,0.,0.));
#2100=DIRECTION('center_axis',(0.,-1.,0.));
#2101=DIRECTION('ref_axis',(1.,0.,0.));
#2102=DIRECTION('center_axis',(0.,-1.,0.));
#2103=DIRECTION('ref_axis',(1.,0.,0.));
#2104=DIRECTION('',(0.,1.,0.));
#2105=DIRECTION('center_axis',(0.,-1.,0.));
#2106=DIRECTION('ref_axis',(1.,0.,0.));
#2107=DIRECTION('center_axis',(0.,-1.,0.));
#2108=DIRECTION('ref_axis',(1.,0.,0.));
#2109=DIRECTION('center_axis',(0.,-1.,0.));
#2110=DIRECTION('ref_axis',(1.,0.,0.));
#2111=DIRECTION('',(0.,0.,1.));
#2112=DIRECTION('',(1.,0.,0.));
#2113=DIRECTION('',(0.,0.,1.));
#2114=DIRECTION('',(1.,0.,0.));
#2115=DIRECTION('',(0.,0.,1.));
#2116=DIRECTION('',(1.,0.,0.));
#2117=DIRECTION('',(0.,0.,1.));
#2118=DIRECTION('',(1.,0.,0.));
#2119=DIRECTION('',(0.,0.,1.));
#2120=DIRECTION('',(1.,0.,0.));
#2121=DIRECTION('',(0.,0.,1.));
#2122=DIRECTION('',(1.,0.,0.));
#2123=DIRECTION('',(0.,0.,1.));
#2124=DIRECTION('',(1.,0.,0.));
#2125=DIRECTION('',(0.,0.,1.));
#2126=DIRECTION('',(1.,0.,0.));
#2127=CARTESIAN_POINT('',(0.,0.,0.));
#2128=CARTESIAN_POINT('',(0.,0.,0.));
#2129=CARTESIAN_POINT('Origin',(-33.3281551220004,0.,66.411927135393));
#2130=CARTESIAN_POINT('',(-33.3724763544127,0.,66.4375215521063));
#2131=CARTESIAN_POINT('',(-33.3724763544127,-10.,66.4375215521063));
#2132=CARTESIAN_POINT('',(-33.3724763544127,0.,66.4375215521063));
#2133=CARTESIAN_POINT('',(-37.4153984446205,0.,68.7722091743641));
#2134=CARTESIAN_POINT('',(-33.3281551220004,0.,66.411927135393));
#2135=CARTESIAN_POINT('',(-37.4153984446205,-10.,68.7722091743641));
#2136=CARTESIAN_POINT('',(-37.4153984446205,0.,68.7722091743641));
#2137=CARTESIAN_POINT('',(-33.3281551220004,-10.,66.411927135393));
#2138=CARTESIAN_POINT('Origin',(-0.957463170361006,0.,59.9988083494084));
#2139=CARTESIAN_POINT('',(-37.9507118793475,-10.,53.8625915627806));
#2140=CARTESIAN_POINT('',(-37.9507118793475,0.,53.8625915627806));
#2141=CARTESIAN_POINT('',(-37.9507118793475,0.,53.8625915627806));
#2142=CARTESIAN_POINT('Origin',(-0.957463170361006,-10.,59.9988083494084));
#2143=CARTESIAN_POINT('Origin',(-0.957463170361006,0.,59.9988083494084));
#2144=CARTESIAN_POINT('Origin',(-37.900309738233,0.,53.8536994325238));
#2145=CARTESIAN_POINT('',(-42.5483261291134,0.,54.673719500509));
#2146=CARTESIAN_POINT('',(-37.900309738233,0.,53.8536994325238));
#2147=CARTESIAN_POINT('',(-42.5483261291134,-10.,54.673719500509));
#2148=CARTESIAN_POINT('',(-42.5483261291134,0.,54.673719500509));
#2149=CARTESIAN_POINT('',(-37.900309738233,-10.,53.8536994325238));
#2150=CARTESIAN_POINT('Origin',(-0.00360820116592997,0.,47.167824608198));
#2151=CARTESIAN_POINT('',(-27.7700567175474,0.,80.2648912227814));
#2152=CARTESIAN_POINT('Origin',(3.48851622115957,0.,59.5512429605134));
#2153=CARTESIAN_POINT('',(-24.7694628581521,0.,76.6882416995582));
#2154=CARTESIAN_POINT('',(-24.7365683291828,0.,76.6490320607774));
#2155=CARTESIAN_POINT('',(-14.7756715102625,0.,87.7655785767993));
#2156=CARTESIAN_POINT('Origin',(7.51329386908021,0.,57.6100545585387));
#2157=CARTESIAN_POINT('',(-13.1793217851717,0.,83.3783638708365));
#2158=CARTESIAN_POINT('',(-13.1618215253105,0.,83.3302682710978));
#2159=CARTESIAN_POINT('',(0.000442544535028677,0.,90.3695776431675));
#2160=CARTESIAN_POINT('Origin',(10.6314221896698,0.,54.4093791136522));
#2161=CARTESIAN_POINT('',(4.79886261666655E-6,0.,85.7009605963974));
#2162=CARTESIAN_POINT('',(0.,0.,85.6497800748447));
#2163=CARTESIAN_POINT('',(14.7760680196183,0.,87.7628077035488));
#2164=CARTESIAN_POINT('Origin',(12.4668088887924,0.,50.3352653214458));
#2165=CARTESIAN_POINT('',(13.1788956017712,0.,83.3758924332613));
#2166=CARTESIAN_POINT('',(13.1613863229985,0.,83.327800116138));
#2167=CARTESIAN_POINT('',(27.769046417685,0.,80.2596836844883));
#2168=CARTESIAN_POINT('Origin',(12.7980792431109,0.,45.8791114327754));
#2169=CARTESIAN_POINT('',(24.7677818930099,0.,76.6835969162539));
#2170=CARTESIAN_POINT('',(24.7348800117566,0.,76.644393446772));
#2171=CARTESIAN_POINT('',(37.4122327879896,0.,68.7651930770015));
#2172=CARTESIAN_POINT('Origin',(11.5852771588649,0.,41.5783953724418));
#2173=CARTESIAN_POINT('',(33.3688729521094,0.,66.4312636524891));
#2174=CARTESIAN_POINT('',(33.3245469208345,0.,66.4056775476497));
#2175=CARTESIAN_POINT('',(42.5425165359998,0.,54.6657410889655));
#2176=CARTESIAN_POINT('Origin',(8.97468446646684,0.,37.9518469691304));
#2177=CARTESIAN_POINT('',(37.9447502587574,0.,53.8554753419011));
#2178=CARTESIAN_POINT('',(37.8943464510154,0.,53.8465926635586));
#2179=CARTESIAN_POINT('',(42.5411097267815,0.,39.661929715887));
#2180=CARTESIAN_POINT('Origin',(5.28117717286475,0.,35.4368814824347));
#2181=CARTESIAN_POINT('',(37.9434954770157,0.,40.4730576536155));
#2182=CARTESIAN_POINT('',(37.8930933359011,0.,40.4819497838722));
#2183=CARTESIAN_POINT('',(37.4081820422886,0.,25.563440042032));
#2184=CARTESIAN_POINT('Origin',(0.950246768029155,0.,34.3368408669877));
#2185=CARTESIAN_POINT('',(33.3652599520808,0.,27.8981276642898));
#2186=CARTESIAN_POINT('',(33.3209387196686,0.,27.923722081003));
#2187=CARTESIAN_POINT('',(27.7628403152156,0.,14.0707579936147));
#2188=CARTESIAN_POINT('Origin',(-3.49573262349144,0.,34.7844062558827));
#2189=CARTESIAN_POINT('',(24.7622464558202,0.,17.6474075168379));
#2190=CARTESIAN_POINT('',(24.7293519268509,0.,17.6866171556187));
#2191=CARTESIAN_POINT('',(14.7684551079306,0.,6.57007063959682));
#2192=CARTESIAN_POINT('Origin',(-7.52051027141208,0.,36.7255946578574));
#2193=CARTESIAN_POINT('',(13.1721053828398,0.,10.9572853455596));
#2194=CARTESIAN_POINT('',(13.1546051229786,0.,11.0053809452983));
#2195=CARTESIAN_POINT('',(-0.00765894686688301,0.,3.9660715732286));
#2196=CARTESIAN_POINT('Origin',(-10.6386385920017,0.,39.9262701027439));
#2197=CARTESIAN_POINT('',(-0.00722120119447005,0.,8.63468861999872));
#2198=CARTESIAN_POINT('',(-0.00721640233185491,0.,8.68586914155136));
#2199=CARTESIAN_POINT('',(-14.7832844219502,0.,6.57284151284728));
#2200=CARTESIAN_POINT('Origin',(-12.4740252911242,0.,44.0003838949503));
#2201=CARTESIAN_POINT('',(-13.1861120041031,0.,10.9597567831348));
#2202=CARTESIAN_POINT('',(-13.1686027253304,0.,11.0078491002581));
#2203=CARTESIAN_POINT('',(-27.7762628200168,0.,14.0759655319078));
#2204=CARTESIAN_POINT('Origin',(-12.8052956454428,0.,48.4565377836207));
#2205=CARTESIAN_POINT('',(-24.7749982953418,0.,17.6520523001422));
#2206=CARTESIAN_POINT('',(-24.7420964140884,0.,17.6912557696241));
#2207=CARTESIAN_POINT('',(-37.4194491903214,0.,25.5704561393946));
#2208=CARTESIAN_POINT('Origin',(-11.5924935611967,0.,52.7572538439543));
#2209=CARTESIAN_POINT('',(-33.3760893544412,0.,27.904385563907));
#2210=CARTESIAN_POINT('',(-33.3317633231664,0.,27.9299716687463));
#2211=CARTESIAN_POINT('',(-42.5497329383317,0.,39.6699081274306));
#2212=CARTESIAN_POINT('Origin',(-8.9819008687987,0.,56.3838022472657));
#2213=CARTESIAN_POINT('',(-37.9519666610893,0.,40.480173874495));
#2214=CARTESIAN_POINT('',(-37.9015628533472,0.,40.4890565528375));
#2215=CARTESIAN_POINT('Origin',(-5.28839357519661,0.,58.8987677339614));
#2216=CARTESIAN_POINT('',(-14.4855638369713,0.,47.167824608198));
#2217=CARTESIAN_POINT('Origin',(-0.00360820116592981,0.,47.167824608198));
#2218=CARTESIAN_POINT('Origin',(-37.9015628533472,0.,40.4890565528375));
#2219=CARTESIAN_POINT('',(-37.9519666610893,-10.,40.480173874495));
#2220=CARTESIAN_POINT('',(-37.9519666610893,0.,40.480173874495));
#2221=CARTESIAN_POINT('',(-42.5497329383317,-10.,39.6699081274306));
#2222=CARTESIAN_POINT('',(-42.5497329383317,0.,39.6699081274306));
#2223=CARTESIAN_POINT('',(-37.9015628533472,-10.,40.4890565528375));
#2224=CARTESIAN_POINT('Origin',(-8.9819008687987,0.,56.3838022472657));
#2225=CARTESIAN_POINT('',(-33.3760893544412,-10.,27.904385563907));
#2226=CARTESIAN_POINT('',(-33.3760893544412,0.,27.904385563907));
#2227=CARTESIAN_POINT('Origin',(-8.9819008687987,-10.,56.3838022472657));
#2228=CARTESIAN_POINT('Origin',(-33.3317633231664,0.,27.9299716687463));
#2229=CARTESIAN_POINT('',(-37.4194491903214,-10.,25.5704561393946));
#2230=CARTESIAN_POINT('',(-37.4194491903214,0.,25.5704561393946));
#2231=CARTESIAN_POINT('',(-33.3317633231664,-10.,27.9299716687463));
#2232=CARTESIAN_POINT('Origin',(-13.1686027253304,0.,11.0078491002581));
#2233=CARTESIAN_POINT('',(-13.1861120041031,-10.,10.9597567831348));
#2234=CARTESIAN_POINT('',(-13.1861120041031,0.,10.9597567831348));
#2235=CARTESIAN_POINT('',(-14.7832844219502,-10.,6.57284151284728));
#2236=CARTESIAN_POINT('',(-14.7832844219502,0.,6.57284151284728));
#2237=CARTESIAN_POINT('',(-13.1686027253304,-10.,11.0078491002581));
#2238=CARTESIAN_POINT('Origin',(-12.4740252911242,0.,44.0003838949503));
#2239=CARTESIAN_POINT('',(-0.00722120119447227,-10.,8.63468861999872));
#2240=CARTESIAN_POINT('',(-0.00722120119447227,0.,8.63468861999872));
#2241=CARTESIAN_POINT('Origin',(-12.4740252911242,-10.,44.0003838949503));
#2242=CARTESIAN_POINT('Origin',(-0.00721640233185491,0.,8.68586914155136));
#2243=CARTESIAN_POINT('',(-0.00765894686688301,-10.,3.9660715732286));
#2244=CARTESIAN_POINT('',(-0.00765894686688301,0.,3.9660715732286));
#2245=CARTESIAN_POINT('',(-0.00721640233185491,-10.,8.68586914155136));
#2246=CARTESIAN_POINT('Origin',(-5.28839357519661,0.,58.8987677339614));
#2247=CARTESIAN_POINT('Origin',(-5.28839357519661,-10.,58.8987677339614));
#2248=CARTESIAN_POINT('Origin',(-11.5924935611967,0.,52.7572538439543));
#2249=CARTESIAN_POINT('',(-24.7749982953418,-10.,17.6520523001422));
#2250=CARTESIAN_POINT('',(-24.7749982953418,0.,17.6520523001422));
#2251=CARTESIAN_POINT('Origin',(-11.5924935611967,-10.,52.7572538439543));
#2252=CARTESIAN_POINT('Origin',(-12.8052956454428,0.,48.4565377836207));
#2253=CARTESIAN_POINT('',(-27.7762628200168,-10.,14.0759655319078));
#2254=CARTESIAN_POINT('Origin',(-12.8052956454428,-10.,48.4565377836207));
#2255=CARTESIAN_POINT('',(-27.7762628200168,0.,14.0759655319078));
#2256=CARTESIAN_POINT('Origin',(-24.7420964140884,0.,17.6912557696241));
#2257=CARTESIAN_POINT('',(-24.7420964140884,-10.,17.6912557696241));
#2258=CARTESIAN_POINT('Origin',(7.51329386908021,0.,57.6100545585387));
#2259=CARTESIAN_POINT('',(-24.7694628581521,-10.,76.6882416995582));
#2260=CARTESIAN_POINT('',(-24.7694628581521,0.,76.6882416995582));
#2261=CARTESIAN_POINT('',(-14.7756715102625,-10.,87.7655785767993));
#2262=CARTESIAN_POINT('Origin',(7.51329386908021,-10.,57.6100545585387));
#2263=CARTESIAN_POINT('',(-14.7756715102625,0.,87.7655785767993));
#2264=CARTESIAN_POINT('Origin',(-13.1618215253105,0.,83.3302682710978));
#2265=CARTESIAN_POINT('',(-13.1793217851717,-10.,83.3783638708365));
#2266=CARTESIAN_POINT('',(-13.1793217851717,0.,83.3783638708365));
#2267=CARTESIAN_POINT('',(-13.1618215253105,-10.,83.3302682710978));
#2268=CARTESIAN_POINT('Origin',(10.6314221896698,0.,54.4093791136522));
#2269=CARTESIAN_POINT('',(0.000442544535028677,-10.,90.3695776431675));
#2270=CARTESIAN_POINT('Origin',(10.6314221896698,-10.,54.4093791136522));
#2271=CARTESIAN_POINT('',(0.000442544535028677,0.,90.3695776431675));
#2272=CARTESIAN_POINT('Origin',(-10.6386385920017,0.,39.9262701027439));
#2273=CARTESIAN_POINT('',(13.1721053828398,-10.,10.9572853455596));
#2274=CARTESIAN_POINT('',(13.1721053828398,0.,10.9572853455596));
#2275=CARTESIAN_POINT('Origin',(-10.6386385920017,-10.,39.9262701027439));
#2276=CARTESIAN_POINT('Origin',(3.48851622115957,0.,59.5512429605134));
#2277=CARTESIAN_POINT('',(-27.7700567175474,-10.,80.2648912227814));
#2278=CARTESIAN_POINT('Origin',(3.48851622115957,-10.,59.5512429605134));
#2279=CARTESIAN_POINT('',(-27.7700567175474,0.,80.2648912227814));
#2280=CARTESIAN_POINT('Origin',(-24.7365683291828,0.,76.6490320607774));
#2281=CARTESIAN_POINT('',(-24.7365683291828,-10.,76.6490320607774));
#2282=CARTESIAN_POINT('Origin',(12.4668088887924,0.,50.3352653214458));
#2283=CARTESIAN_POINT('',(4.79886261666655E-6,-10.,85.7009605963974));
#2284=CARTESIAN_POINT('',(4.798862618887E-6,0.,85.7009605963974));
#2285=CARTESIAN_POINT('',(14.7760680196183,-10.,87.7628077035488));
#2286=CARTESIAN_POINT('Origin',(12.4668088887924,-10.,50.3352653214458));
#2287=CARTESIAN_POINT('',(14.7760680196183,0.,87.7628077035488));
#2288=CARTESIAN_POINT('Origin',(13.1613863229985,0.,83.327800116138));
#2289=CARTESIAN_POINT('',(13.1788956017712,-10.,83.3758924332613));
#2290=CARTESIAN_POINT('',(13.1788956017712,0.,83.3758924332613));
#2291=CARTESIAN_POINT('',(13.1613863229985,-10.,83.327800116138));
#2292=CARTESIAN_POINT('Origin',(8.97468446646684,0.,37.9518469691304));
#2293=CARTESIAN_POINT('',(33.3688729521094,-10.,66.4312636524891));
#2294=CARTESIAN_POINT('',(33.3688729521094,0.,66.4312636524891));
#2295=CARTESIAN_POINT('',(42.5425165359998,-10.,54.6657410889655));
#2296=CARTESIAN_POINT('Origin',(8.97468446646684,-10.,37.9518469691304));
#2297=CARTESIAN_POINT('',(42.5425165359998,0.,54.6657410889655));
#2298=CARTESIAN_POINT('Origin',(37.8943464510154,0.,53.8465926635586));
#2299=CARTESIAN_POINT('',(37.9447502587574,-10.,53.8554753419011));
#2300=CARTESIAN_POINT('',(37.9447502587574,0.,53.8554753419011));
#2301=CARTESIAN_POINT('',(37.8943464510154,-10.,53.8465926635586));
#2302=CARTESIAN_POINT('Origin',(5.28117717286475,0.,35.4368814824347));
#2303=CARTESIAN_POINT('',(42.5411097267815,-10.,39.661929715887));
#2304=CARTESIAN_POINT('Origin',(5.28117717286475,-10.,35.4368814824347));
#2305=CARTESIAN_POINT('',(42.5411097267815,0.,39.661929715887));
#2306=CARTESIAN_POINT('Origin',(-0.00360820116592997,-10.,47.167824608198));
#2307=CARTESIAN_POINT('',(14.7684551079306,-10.,6.57007063959682));
#2308=CARTESIAN_POINT('',(13.1546051229786,-10.,11.0053809452983));
#2309=CARTESIAN_POINT('',(24.7622464558202,-10.,17.6474075168379));
#2310=CARTESIAN_POINT('Origin',(-7.52051027141208,-10.,36.7255946578574));
#2311=CARTESIAN_POINT('',(27.7628403152156,-10.,14.0707579936147));
#2312=CARTESIAN_POINT('',(24.7293519268509,-10.,17.6866171556187));
#2313=CARTESIAN_POINT('',(33.3652599520808,-10.,27.8981276642898));
#2314=CARTESIAN_POINT('Origin',(-3.49573262349144,-10.,34.7844062558827));
#2315=CARTESIAN_POINT('',(37.4081820422886,-10.,25.563440042032));
#2316=CARTESIAN_POINT('',(33.3209387196686,-10.,27.923722081003));
#2317=CARTESIAN_POINT('',(37.9434954770157,-10.,40.4730576536155));
#2318=CARTESIAN_POINT('Origin',(0.950246768029155,-10.,34.3368408669877));
#2319=CARTESIAN_POINT('',(37.8930933359011,-10.,40.4819497838722));
#2320=CARTESIAN_POINT('',(37.4122327879896,-10.,68.7651930770015));
#2321=CARTESIAN_POINT('',(33.3245469208345,-10.,66.4056775476497));
#2322=CARTESIAN_POINT('',(24.7677818930099,-10.,76.6835969162539));
#2323=CARTESIAN_POINT('Origin',(11.5852771588649,-10.,41.5783953724418));
#2324=CARTESIAN_POINT('',(27.769046417685,-10.,80.2596836844883));
#2325=CARTESIAN_POINT('',(24.7348800117566,-10.,76.644393446772));
#2326=CARTESIAN_POINT('Origin',(12.7980792431109,-10.,45.8791114327754));
#2327=CARTESIAN_POINT('',(0.,-10.,85.6497800748447));
#2328=CARTESIAN_POINT('',(-14.4855638369713,-10.,47.167824608198));
#2329=CARTESIAN_POINT('Origin',(-0.00360820116592981,-10.,47.167824608198));
#2330=CARTESIAN_POINT('Origin',(11.5852771588649,0.,41.5783953724418));
#2331=CARTESIAN_POINT('',(24.7677818930099,0.,76.6835969162539));
#2332=CARTESIAN_POINT('',(37.4122327879896,0.,68.7651930770015));
#2333=CARTESIAN_POINT('Origin',(33.3245469208345,0.,66.4056775476497));
#2334=CARTESIAN_POINT('Origin',(12.7980792431109,0.,45.8791114327754));
#2335=CARTESIAN_POINT('',(27.769046417685,0.,80.2596836844883));
#2336=CARTESIAN_POINT('Origin',(24.7348800117566,0.,76.644393446772));
#2337=CARTESIAN_POINT('Origin',(33.3209387196686,0.,27.923722081003));
#2338=CARTESIAN_POINT('',(33.3652599520808,0.,27.8981276642898));
#2339=CARTESIAN_POINT('',(37.4081820422886,0.,25.563440042032));
#2340=CARTESIAN_POINT('Origin',(0.950246768029155,0.,34.3368408669877));
#2341=CARTESIAN_POINT('',(37.9434954770157,0.,40.4730576536155));
#2342=CARTESIAN_POINT('Origin',(37.8930933359011,0.,40.4819497838722));
#2343=CARTESIAN_POINT('Origin',(-7.52051027141208,0.,36.7255946578574));
#2344=CARTESIAN_POINT('',(24.7622464558202,0.,17.6474075168379));
#2345=CARTESIAN_POINT('',(14.7684551079306,0.,6.57007063959682));
#2346=CARTESIAN_POINT('Origin',(13.1546051229786,0.,11.0053809452983));
#2347=CARTESIAN_POINT('Origin',(-3.49573262349144,0.,34.7844062558827));
#2348=CARTESIAN_POINT('',(27.7628403152156,0.,14.0707579936147));
#2349=CARTESIAN_POINT('Origin',(24.7293519268509,0.,17.6866171556187));
#2350=CARTESIAN_POINT('Origin',(0.,0.,85.6497800748447));
#2351=CARTESIAN_POINT('Origin',(-0.00360820116592981,0.,47.167824608198));
#2352=CARTESIAN_POINT('',(-14.4855638369713,0.,47.167824608198));
#2353=CARTESIAN_POINT('',(0.,0.,0.));
#2354=CARTESIAN_POINT('Origin',(73.2288574389116,0.,87.4952777324745));
#2355=CARTESIAN_POINT('',(67.2288574389116,0.,87.4952777324745));
#2356=CARTESIAN_POINT('Origin',(73.2288574389116,0.,87.4952777324745));
#2357=CARTESIAN_POINT('',(67.2288574389116,-10.,87.4952777324745));
#2358=CARTESIAN_POINT('',(67.2288574389116,0.,87.4952777324745));
#2359=CARTESIAN_POINT('Origin',(73.2288574389116,-10.,87.4952777324745));
#2360=CARTESIAN_POINT('Ctrl Pts',(78.5565765069325,0.,96.7614764365663));
#2361=CARTESIAN_POINT('Ctrl Pts',(78.5565765069325,-10.,96.7614764365663));
#2362=CARTESIAN_POINT('Ctrl Pts',(77.933781500681,0.,97.1195603646402));
#2363=CARTESIAN_POINT('Ctrl Pts',(77.933781500681,-10.,97.1195603646402));
#2364=CARTESIAN_POINT('Ctrl Pts',(76.6526666483233,0.,97.7826386838039));
#2365=CARTESIAN_POINT('Ctrl Pts',(76.6526666483233,-10.,97.7826386838039));
#2366=CARTESIAN_POINT('Ctrl Pts',(74.6244214366979,0.,98.6179893838346));
#2367=CARTESIAN_POINT('Ctrl Pts',(74.6244214366979,-10.,98.6179893838346));
#2368=CARTESIAN_POINT('Ctrl Pts',(71.6890880153669,0.,99.4224704752722));
#2369=CARTESIAN_POINT('Ctrl Pts',(71.6890880153669,-10.,99.4224704752722));
#2370=CARTESIAN_POINT('Ctrl Pts',(67.5475314586935,0.,99.9655376285179));
#2371=CARTESIAN_POINT('Ctrl Pts',(67.5475314586935,-10.,99.9655376285179));
#2372=CARTESIAN_POINT('Ctrl Pts',(62.8494346176935,0.,100.11488638886));
#2373=CARTESIAN_POINT('Ctrl Pts',(62.8494346176935,-10.,100.11488638886));
#2374=CARTESIAN_POINT('Ctrl Pts',(57.5623233061826,0.,99.9423456500588));
#2375=CARTESIAN_POINT('Ctrl Pts',(57.5623233061826,-10.,99.9423456500588));
#2376=CARTESIAN_POINT('Ctrl Pts',(51.7530480696311,0.,99.5113992758897));
#2377=CARTESIAN_POINT('Ctrl Pts',(51.7530480696311,-10.,99.5113992758897));
#2378=CARTESIAN_POINT('Ctrl Pts',(45.5547012575949,0.,98.8769393338912));
#2379=CARTESIAN_POINT('Ctrl Pts',(45.5547012575949,-10.,98.8769393338912));
#2380=CARTESIAN_POINT('Ctrl Pts',(39.1395829757266,0.,98.0850994498989));
#2381=CARTESIAN_POINT('Ctrl Pts',(39.1395829757266,-10.,98.0850994498989));
#2382=CARTESIAN_POINT('Ctrl Pts',(32.6920975126609,0.,97.1735392968004));
#2383=CARTESIAN_POINT('Ctrl Pts',(32.6920975126609,-10.,97.1735392968004));
#2384=CARTESIAN_POINT('Ctrl Pts',(26.384627993242,0.,96.1718956743097));
#2385=CARTESIAN_POINT('Ctrl Pts',(26.384627993242,-10.,96.1718956743097));
#2386=CARTESIAN_POINT('Ctrl Pts',(20.3489626390195,0.,95.1023403943181));
#2387=CARTESIAN_POINT('Ctrl Pts',(20.3489626390195,-10.,95.1023403943181));
#2388=CARTESIAN_POINT('Ctrl Pts',(14.6587606984742,0.,93.9803229433208));
#2389=CARTESIAN_POINT('Ctrl Pts',(14.6587606984742,-10.,93.9803229433208));
#2390=CARTESIAN_POINT('Ctrl Pts',(9.3499076568271,0.,92.8157760857789));
#2391=CARTESIAN_POINT('Ctrl Pts',(9.3499076568271,-10.,92.8157760857789));
#2392=CARTESIAN_POINT('Ctrl Pts',(5.41600698566024,0.,91.854562206062));
#2393=CARTESIAN_POINT('Ctrl Pts',(5.41600698566024,-10.,91.854562206062));
#2394=CARTESIAN_POINT('Ctrl Pts',(2.64064416187385,0.,91.1180813473512));
#2395=CARTESIAN_POINT('Ctrl Pts',(2.64064416187385,-10.,91.1180813473512));
#2396=CARTESIAN_POINT('Ctrl Pts',(0.867636945837178,0.,90.6202239141436));
#2397=CARTESIAN_POINT('Ctrl Pts',(0.867636945837178,-10.,90.6202239141436));
#2398=CARTESIAN_POINT('Ctrl Pts',(0.000442544535028507,0.,90.3695776431675));
#2399=CARTESIAN_POINT('Ctrl Pts',(0.000442544535028507,-10.,90.3695776431675));
#2400=CARTESIAN_POINT('',(0.000442544535028507,0.,90.3695776431675));
#2401=CARTESIAN_POINT('',(78.5565765069325,0.,96.7614764365663));
#2402=CARTESIAN_POINT('Ctrl Pts',(0.000442544535028507,0.,90.3695776431675));
#2403=CARTESIAN_POINT('Ctrl Pts',(0.867636945837178,0.,90.6202239141436));
#2404=CARTESIAN_POINT('Ctrl Pts',(2.64064416187385,0.,91.1180813473512));
#2405=CARTESIAN_POINT('Ctrl Pts',(5.41600698566024,0.,91.854562206062));
#2406=CARTESIAN_POINT('Ctrl Pts',(9.3499076568271,0.,92.8157760857789));
#2407=CARTESIAN_POINT('Ctrl Pts',(14.6587606984742,0.,93.9803229433208));
#2408=CARTESIAN_POINT('Ctrl Pts',(20.3489626390195,0.,95.1023403943181));
#2409=CARTESIAN_POINT('Ctrl Pts',(26.384627993242,0.,96.1718956743097));
#2410=CARTESIAN_POINT('Ctrl Pts',(32.6920975126609,0.,97.1735392968004));
#2411=CARTESIAN_POINT('Ctrl Pts',(39.1395829757266,0.,98.0850994498989));
#2412=CARTESIAN_POINT('Ctrl Pts',(45.5547012575949,0.,98.8769393338912));
#2413=CARTESIAN_POINT('Ctrl Pts',(51.7530480696311,0.,99.5113992758897));
#2414=CARTESIAN_POINT('Ctrl Pts',(57.5623233061826,0.,99.9423456500588));
#2415=CARTESIAN_POINT('Ctrl Pts',(62.8494346176935,0.,100.11488638886));
#2416=CARTESIAN_POINT('Ctrl Pts',(67.5475314586935,0.,99.9655376285179));
#2417=CARTESIAN_POINT('Ctrl Pts',(71.6890880153669,0.,99.4224704752722));
#2418=CARTESIAN_POINT('Ctrl Pts',(74.6244214366979,0.,98.6179893838346));
#2419=CARTESIAN_POINT('Ctrl Pts',(76.6526666483233,0.,97.7826386838039));
#2420=CARTESIAN_POINT('Ctrl Pts',(77.933781500681,0.,97.1195603646402));
#2421=CARTESIAN_POINT('Ctrl Pts',(78.5565765069325,0.,96.7614764365663));
#2422=CARTESIAN_POINT('',(0.000442544535028507,-10.,90.3695776431675));
#2423=CARTESIAN_POINT('',(0.000442544535028507,0.,90.3695776431675));
#2424=CARTESIAN_POINT('',(78.5565765069325,-10.,96.7614764365663));
#2425=CARTESIAN_POINT('Ctrl Pts',(78.5565765069325,-10.,96.7614764365663));
#2426=CARTESIAN_POINT('Ctrl Pts',(77.933781500681,-10.,97.1195603646402));
#2427=CARTESIAN_POINT('Ctrl Pts',(76.6526666483233,-10.,97.7826386838039));
#2428=CARTESIAN_POINT('Ctrl Pts',(74.6244214366979,-10.,98.6179893838346));
#2429=CARTESIAN_POINT('Ctrl Pts',(71.6890880153669,-10.,99.4224704752722));
#2430=CARTESIAN_POINT('Ctrl Pts',(67.5475314586935,-10.,99.9655376285179));
#2431=CARTESIAN_POINT('Ctrl Pts',(62.8494346176935,-10.,100.11488638886));
#2432=CARTESIAN_POINT('Ctrl Pts',(57.5623233061826,-10.,99.9423456500588));
#2433=CARTESIAN_POINT('Ctrl Pts',(51.7530480696311,-10.,99.5113992758897));
#2434=CARTESIAN_POINT('Ctrl Pts',(45.5547012575949,-10.,98.8769393338912));
#2435=CARTESIAN_POINT('Ctrl Pts',(39.1395829757266,-10.,98.0850994498989));
#2436=CARTESIAN_POINT('Ctrl Pts',(32.6920975126609,-10.,97.1735392968004));
#2437=CARTESIAN_POINT('Ctrl Pts',(26.384627993242,-10.,96.1718956743097));
#2438=CARTESIAN_POINT('Ctrl Pts',(20.3489626390195,-10.,95.1023403943181));
#2439=CARTESIAN_POINT('Ctrl Pts',(14.6587606984742,-10.,93.9803229433208));
#2440=CARTESIAN_POINT('Ctrl Pts',(9.3499076568271,-10.,92.8157760857789));
#2441=CARTESIAN_POINT('Ctrl Pts',(5.41600698566024,-10.,91.854562206062));
#2442=CARTESIAN_POINT('Ctrl Pts',(2.64064416187385,-10.,91.1180813473512));
#2443=CARTESIAN_POINT('Ctrl Pts',(0.867636945837178,-10.,90.6202239141436));
#2444=CARTESIAN_POINT('Ctrl Pts',(0.000442544535028507,-10.,90.3695776431675));
#2445=CARTESIAN_POINT('',(78.5565765069325,0.,96.7614764365663));
#2446=CARTESIAN_POINT('Origin',(73.2288574389116,0.,87.4952777324745));
#2447=CARTESIAN_POINT('',(73.7249441578369,0.,76.8181560763928));
#2448=CARTESIAN_POINT('Origin',(73.2288574389116,0.,87.4952777324745));
#2449=CARTESIAN_POINT('',(73.7249441578369,-10.,76.8181560763928));
#2450=CARTESIAN_POINT('Origin',(73.2288574389116,-10.,87.4952777324745));
#2451=CARTESIAN_POINT('',(73.7249441578369,0.,76.8181560763928));
#2452=CARTESIAN_POINT('Ctrl Pts',(14.7760680196183,0.,87.7628077035488));
#2453=CARTESIAN_POINT('Ctrl Pts',(14.7760680196183,-10.,87.7628077035488));
#2454=CARTESIAN_POINT('Ctrl Pts',(15.2822994559612,0.,87.7315734976063));
#2455=CARTESIAN_POINT('Ctrl Pts',(15.2822994559612,-10.,87.7315734976063));
#2456=CARTESIAN_POINT('Ctrl Pts',(16.2934759211885,0.,87.669785304704));
#2457=CARTESIAN_POINT('Ctrl Pts',(16.2934759211885,-10.,87.669785304704));
#2458=CARTESIAN_POINT('Ctrl Pts',(17.8063864959714,0.,87.5791386198598));
#2459=CARTESIAN_POINT('Ctrl Pts',(17.8063864959714,-10.,87.5791386198598));
#2460=CARTESIAN_POINT('Ctrl Pts',(19.8250496559672,0.,87.4534593828614));
#2461=CARTESIAN_POINT('Ctrl Pts',(19.8250496559672,-10.,87.4534593828614));
#2462=CARTESIAN_POINT('Ctrl Pts',(22.4011592565578,0.,87.2395858399089));
#2463=CARTESIAN_POINT('Ctrl Pts',(22.4011592565578,-10.,87.2395858399089));
#2464=CARTESIAN_POINT('Ctrl Pts',(25.0887629856102,0.,86.9124001611246));
#2465=CARTESIAN_POINT('Ctrl Pts',(25.0887629856102,-10.,86.9124001611246));
#2466=CARTESIAN_POINT('Ctrl Pts',(27.9380040884934,0.,86.4241239702294));
#2467=CARTESIAN_POINT('Ctrl Pts',(27.9380040884934,-10.,86.4241239702294));
#2468=CARTESIAN_POINT('Ctrl Pts',(30.9683248537247,0.,85.75747543975));
#2469=CARTESIAN_POINT('Ctrl Pts',(30.9683248537247,-10.,85.75747543975));
#2470=CARTESIAN_POINT('Ctrl Pts',(34.165400944085,0.,84.928453366817));
#2471=CARTESIAN_POINT('Ctrl Pts',(34.165400944085,-10.,84.928453366817));
#2472=CARTESIAN_POINT('Ctrl Pts',(37.4932382987616,0.,83.9740394198894));
#2473=CARTESIAN_POINT('Ctrl Pts',(37.4932382987616,-10.,83.9740394198894));
#2474=CARTESIAN_POINT('Ctrl Pts',(40.9013700189392,0.,82.9447683400012));
#2475=CARTESIAN_POINT('Ctrl Pts',(40.9013700189392,-10.,82.9447683400012));
#2476=CARTESIAN_POINT('Ctrl Pts',(44.3336493923615,0.,81.8956839784984));
#2477=CARTESIAN_POINT('Ctrl Pts',(44.3336493923615,-10.,81.8956839784984));
#2478=CARTESIAN_POINT('Ctrl Pts',(47.7360606768338,0.,80.8782861138939));
#2479=CARTESIAN_POINT('Ctrl Pts',(47.7360606768338,-10.,80.8782861138939));
#2480=CARTESIAN_POINT('Ctrl Pts',(51.0650378422273,0.,79.9318697713207));
#2481=CARTESIAN_POINT('Ctrl Pts',(51.0650378422273,-10.,79.9318697713207));
#2482=CARTESIAN_POINT('Ctrl Pts',(54.288048859871,0.,79.085110401947));
#2483=CARTESIAN_POINT('Ctrl Pts',(54.288048859871,-10.,79.085110401947));
#2484=CARTESIAN_POINT('Ctrl Pts',(57.3840999328369,0.,78.357680633469));
#2485=CARTESIAN_POINT('Ctrl Pts',(57.3840999328369,-10.,78.357680633469));
#2486=CARTESIAN_POINT('Ctrl Pts',(60.3448286085174,0.,77.7615650133373));
#2487=CARTESIAN_POINT('Ctrl Pts',(60.3448286085174,-10.,77.7615650133373));
#2488=CARTESIAN_POINT('Ctrl Pts',(63.175078635463,0.,77.3023279219762));
#2489=CARTESIAN_POINT('Ctrl Pts',(63.175078635463,-10.,77.3023279219762));
#2490=CARTESIAN_POINT('Ctrl Pts',(65.8955912826513,0.,76.9799168209156));
#2491=CARTESIAN_POINT('Ctrl Pts',(65.8955912826513,-10.,76.9799168209156));
#2492=CARTESIAN_POINT('Ctrl Pts',(68.5390245353947,0.,76.7903239063253));
#2493=CARTESIAN_POINT('Ctrl Pts',(68.5390245353947,-10.,76.7903239063253));
#2494=CARTESIAN_POINT('Ctrl Pts',(70.619638872722,0.,76.7404944287697));
#2495=CARTESIAN_POINT('Ctrl Pts',(70.619638872722,-10.,76.7404944287697));
#2496=CARTESIAN_POINT('Ctrl Pts',(72.1734485372099,0.,76.7581820414634));
#2497=CARTESIAN_POINT('Ctrl Pts',(72.1734485372099,-10.,76.7581820414634));
#2498=CARTESIAN_POINT('Ctrl Pts',(73.2079991529442,0.,76.7941374729149));
#2499=CARTESIAN_POINT('Ctrl Pts',(73.2079991529442,-10.,76.7941374729149));
#2500=CARTESIAN_POINT('Ctrl Pts',(73.7249441578369,0.,76.8181560763928));
#2501=CARTESIAN_POINT('Ctrl Pts',(73.7249441578369,-10.,76.8181560763928));
#2502=CARTESIAN_POINT('',(14.7760680196183,0.,87.7628077035488));
#2503=CARTESIAN_POINT('Ctrl Pts',(14.7760680196183,0.,87.7628077035488));
#2504=CARTESIAN_POINT('Ctrl Pts',(15.2822994559612,0.,87.7315734976063));
#2505=CARTESIAN_POINT('Ctrl Pts',(16.2934759211885,0.,87.669785304704));
#2506=CARTESIAN_POINT('Ctrl Pts',(17.8063864959714,0.,87.5791386198598));
#2507=CARTESIAN_POINT('Ctrl Pts',(19.8250496559672,0.,87.4534593828614));
#2508=CARTESIAN_POINT('Ctrl Pts',(22.4011592565578,0.,87.2395858399089));
#2509=CARTESIAN_POINT('Ctrl Pts',(25.0887629856102,0.,86.9124001611246));
#2510=CARTESIAN_POINT('Ctrl Pts',(27.9380040884934,0.,86.4241239702294));
#2511=CARTESIAN_POINT('Ctrl Pts',(30.9683248537247,0.,85.75747543975));
#2512=CARTESIAN_POINT('Ctrl Pts',(34.165400944085,0.,84.928453366817));
#2513=CARTESIAN_POINT('Ctrl Pts',(37.4932382987616,0.,83.9740394198894));
#2514=CARTESIAN_POINT('Ctrl Pts',(40.9013700189392,0.,82.9447683400012));
#2515=CARTESIAN_POINT('Ctrl Pts',(44.3336493923615,0.,81.8956839784984));
#2516=CARTESIAN_POINT('Ctrl Pts',(47.7360606768338,0.,80.8782861138939));
#2517=CARTESIAN_POINT('Ctrl Pts',(51.0650378422273,0.,79.9318697713207));
#2518=CARTESIAN_POINT('Ctrl Pts',(54.288048859871,0.,79.085110401947));
#2519=CARTESIAN_POINT('Ctrl Pts',(57.3840999328369,0.,78.357680633469));
#2520=CARTESIAN_POINT('Ctrl Pts',(60.3448286085174,0.,77.7615650133373));
#2521=CARTESIAN_POINT('Ctrl Pts',(63.175078635463,0.,77.3023279219762));
#2522=CARTESIAN_POINT('Ctrl Pts',(65.8955912826513,0.,76.9799168209156));
#2523=CARTESIAN_POINT('Ctrl Pts',(68.5390245353947,0.,76.7903239063253));
#2524=CARTESIAN_POINT('Ctrl Pts',(70.619638872722,0.,76.7404944287697));
#2525=CARTESIAN_POINT('Ctrl Pts',(72.1734485372099,0.,76.7581820414634));
#2526=CARTESIAN_POINT('Ctrl Pts',(73.2079991529442,0.,76.7941374729149));
#2527=CARTESIAN_POINT('Ctrl Pts',(73.7249441578369,0.,76.8181560763928));
#2528=CARTESIAN_POINT('',(14.7760680196183,-10.,87.7628077035488));
#2529=CARTESIAN_POINT('Ctrl Pts',(14.7760680196183,-10.,87.7628077035488));
#2530=CARTESIAN_POINT('Ctrl Pts',(15.2822994559612,-10.,87.7315734976063));
#2531=CARTESIAN_POINT('Ctrl Pts',(16.2934759211885,-10.,87.669785304704));
#2532=CARTESIAN_POINT('Ctrl Pts',(17.8063864959714,-10.,87.5791386198598));
#2533=CARTESIAN_POINT('Ctrl Pts',(19.8250496559672,-10.,87.4534593828614));
#2534=CARTESIAN_POINT('Ctrl Pts',(22.4011592565578,-10.,87.2395858399089));
#2535=CARTESIAN_POINT('Ctrl Pts',(25.0887629856102,-10.,86.9124001611246));
#2536=CARTESIAN_POINT('Ctrl Pts',(27.9380040884934,-10.,86.4241239702294));
#2537=CARTESIAN_POINT('Ctrl Pts',(30.9683248537247,-10.,85.75747543975));
#2538=CARTESIAN_POINT('Ctrl Pts',(34.165400944085,-10.,84.928453366817));
#2539=CARTESIAN_POINT('Ctrl Pts',(37.4932382987616,-10.,83.9740394198894));
#2540=CARTESIAN_POINT('Ctrl Pts',(40.9013700189392,-10.,82.9447683400012));
#2541=CARTESIAN_POINT('Ctrl Pts',(44.3336493923615,-10.,81.8956839784984));
#2542=CARTESIAN_POINT('Ctrl Pts',(47.7360606768338,-10.,80.8782861138939));
#2543=CARTESIAN_POINT('Ctrl Pts',(51.0650378422273,-10.,79.9318697713207));
#2544=CARTESIAN_POINT('Ctrl Pts',(54.288048859871,-10.,79.085110401947));
#2545=CARTESIAN_POINT('Ctrl Pts',(57.3840999328369,-10.,78.357680633469));
#2546=CARTESIAN_POINT('Ctrl Pts',(60.3448286085174,-10.,77.7615650133373));
#2547=CARTESIAN_POINT('Ctrl Pts',(63.175078635463,-10.,77.3023279219762));
#2548=CARTESIAN_POINT('Ctrl Pts',(65.8955912826513,-10.,76.9799168209156));
#2549=CARTESIAN_POINT('Ctrl Pts',(68.5390245353947,-10.,76.7903239063253));
#2550=CARTESIAN_POINT('Ctrl Pts',(70.619638872722,-10.,76.7404944287697));
#2551=CARTESIAN_POINT('Ctrl Pts',(72.1734485372099,-10.,76.7581820414634));
#2552=CARTESIAN_POINT('Ctrl Pts',(73.2079991529442,-10.,76.7941374729149));
#2553=CARTESIAN_POINT('Ctrl Pts',(73.7249441578369,-10.,76.8181560763928));
#2554=CARTESIAN_POINT('',(14.7760680196183,0.,87.7628077035488));
#2555=CARTESIAN_POINT('Origin',(12.4668088887924,0.,50.3352653214454));
#2556=CARTESIAN_POINT('',(4.79886262727547E-6,0.,85.7009605963974));
#2557=CARTESIAN_POINT('Origin',(12.4668088887924,0.,50.3352653214454));
#2558=CARTESIAN_POINT('',(4.79886262727547E-6,-10.,85.7009605963974));
#2559=CARTESIAN_POINT('Origin',(12.4668088887924,-10.,50.3352653214454));
#2560=CARTESIAN_POINT('',(4.79886262727547E-6,0.,85.7009605963974));
#2561=CARTESIAN_POINT('Origin',(0.000442544535028507,0.,90.3695776431675));
#2562=CARTESIAN_POINT('',(0.,0.,85.6497800748447));
#2563=CARTESIAN_POINT('',(0.,-10.,85.6497800748447));
#2564=CARTESIAN_POINT('Origin',(41.9587512087457,0.,88.4276904088147));
#2565=CARTESIAN_POINT('Origin',(41.9587512087457,-10.,88.4276904088147));
#2566=CARTESIAN_POINT('',(0.,0.,0.));
#2567=CARTESIAN_POINT('Ctrl Pts',(56.6181736442213,-16.9999774720125,50.2376372405532));
#2568=CARTESIAN_POINT('Ctrl Pts',(56.6181736442213,-17.5445585268313,50.1654099348961));
#2569=CARTESIAN_POINT('Ctrl Pts',(56.6181736442213,-18.5450363459383,49.9971956031968));
#2570=CARTESIAN_POINT('Ctrl Pts',(56.6181736442213,-19.7685844487136,49.493904422604));
#2571=CARTESIAN_POINT('Ctrl Pts',(56.6181736442213,-20.6981100416586,48.489204295438));
#2572=CARTESIAN_POINT('Ctrl Pts',(56.6181736442214,-21.5561871796402,46.50222984823));
#2573=CARTESIAN_POINT('Ctrl Pts',(56.6181736442213,-21.8921327321723,43.9745858341972));
#2574=CARTESIAN_POINT('Ctrl Pts',(56.6181736442213,-21.8405547289732,41.973830798324));
#2575=CARTESIAN_POINT('Ctrl Pts',(56.6181736442213,-21.7909247107181,41.2895085231153));
#2576=CARTESIAN_POINT('Ctrl Pts',(56.618157657027,-16.9607330396014,49.9417411912163));
#2577=CARTESIAN_POINT('Ctrl Pts',(56.618157657027,-17.4971627471983,49.8705949915618));
#2578=CARTESIAN_POINT('Ctrl Pts',(56.6181576570271,-18.4805860762608,49.7024575220591));
#2579=CARTESIAN_POINT('Ctrl Pts',(56.6181576570271,-19.5946720652724,49.2381096635961));
#2580=CARTESIAN_POINT('Ctrl Pts',(56.6181576570271,-20.4358764482362,48.3351593148684));
#2581=CARTESIAN_POINT('Ctrl Pts',(56.6181576570271,-21.2635356262042,46.4375753069283));
#2582=CARTESIAN_POINT('Ctrl Pts',(56.618157657027,-21.5933664996061,43.9574760043368));
#2583=CARTESIAN_POINT('Ctrl Pts',(56.618157657027,-21.5421903626094,41.9863338279172));
#2584=CARTESIAN_POINT('Ctrl Pts',(56.618157657027,-21.4932194344719,41.3110994004402));
#2585=CARTESIAN_POINT('Ctrl Pts',(56.905319880527,-16.8821224243696,49.3490311160804));
#2586=CARTESIAN_POINT('Ctrl Pts',(56.905319880527,-17.402249022489,49.2800471834769));
#2587=CARTESIAN_POINT('Ctrl Pts',(56.9053198805271,-18.351402212785,49.1122156518553));
#2588=CARTESIAN_POINT('Ctrl Pts',(56.9053198805271,-19.2464726950456,48.7258501952951));
#2589=CARTESIAN_POINT('Ctrl Pts',(56.905319880527,-19.9109000058981,48.0265380482217));
#2590=CARTESIAN_POINT('Ctrl Pts',(56.9053198805271,-20.6776200693149,46.3078832788634));
#2591=CARTESIAN_POINT('Ctrl Pts',(56.905319880527,-20.995035487576,43.9231272443799));
#2592=CARTESIAN_POINT('Ctrl Pts',(56.905319880527,-20.9445380069861,42.0114064070899));
#2593=CARTESIAN_POINT('Ctrl Pts',(56.905319880527,-20.896885292642,41.3543481377929));
#2594=CARTESIAN_POINT('Ctrl Pts',(57.8731003937659,-16.8534555622595,49.1328880679052));
#2595=CARTESIAN_POINT('Ctrl Pts',(57.8731003937659,-17.3675474908954,49.0647045082001));
#2596=CARTESIAN_POINT('Ctrl Pts',(57.873100393766,-18.3045926185379,48.8964381348405));
#2597=CARTESIAN_POINT('Ctrl Pts',(57.873100393766,-19.1189021385899,48.5386005456125));
#2598=CARTESIAN_POINT('Ctrl Pts',(57.873100393766,-19.7183632902904,47.914185411008));
#2599=CARTESIAN_POINT('Ctrl Pts',(57.873100393766,-20.4628924782868,46.2612442706814));
#2600=CARTESIAN_POINT('Ctrl Pts',(57.8731003937659,-20.7763812483859,43.9108746314944));
#2601=CARTESIAN_POINT('Ctrl Pts',(57.8731003937659,-20.7265854309009,42.0204498982018));
#2602=CARTESIAN_POINT('Ctrl Pts',(57.8731003937659,-20.6794206593362,41.370119615811));
#2603=CARTESIAN_POINT('Ctrl Pts',(58.6517637674637,-16.9346108560101,49.7447845670574));
#2604=CARTESIAN_POINT('Ctrl Pts',(58.6517637674637,-17.4656187961995,49.6743574516389));
#2605=CARTESIAN_POINT('Ctrl Pts',(58.6517637674638,-18.4376727944556,49.5062955564888));
#2606=CARTESIAN_POINT('Ctrl Pts',(58.6517637674638,-19.478937649954,49.0678654289268));
#2607=CARTESIAN_POINT('Ctrl Pts',(58.6517637674637,-20.2613753689088,48.2326141213349));
#2608=CARTESIAN_POINT('Ctrl Pts',(58.6517637674638,-21.0687860903838,46.3945101552329));
#2609=CARTESIAN_POINT('Ctrl Pts',(58.6517637674637,-21.3945200169302,43.9460750151473));
#2610=CARTESIAN_POINT('Ctrl Pts',(58.6517637674637,-21.3435910811886,41.9946606461063));
#2611=CARTESIAN_POINT('Ctrl Pts',(58.6517637674637,-21.2950585386603,41.3254708877245));
#2612=CARTESIAN_POINT('Ctrl Pts',(58.6489192212011,-17.0652276031362,50.7296116387549));
#2613=CARTESIAN_POINT('Ctrl Pts',(58.6489192212011,-17.6233774657808,50.6555847140666));
#2614=CARTESIAN_POINT('Ctrl Pts',(58.6489192212011,-18.6521419321212,50.4873396881221));
#2615=CARTESIAN_POINT('Ctrl Pts',(58.6489192212011,-20.0578469197985,49.9192830095945));
#2616=CARTESIAN_POINT('Ctrl Pts',(58.6489192212011,-21.1343096540523,48.7452945362702));
#2617=CARTESIAN_POINT('Ctrl Pts',(58.6489192212011,-22.0429558645062,46.6096118224168));
#2618=CARTESIAN_POINT('Ctrl Pts',(58.648919221201,-22.3889612643844,44.002985085501));
#2619=CARTESIAN_POINT('Ctrl Pts',(58.6489192212011,-22.3366343831035,41.9530602347304));
#2620=CARTESIAN_POINT('Ctrl Pts',(58.6489192212011,-22.2859072373551,41.2536102443029));
#2621=CARTESIAN_POINT('Ctrl Pts',(57.8740741606582,-17.146943550959,51.3457353700218));
#2622=CARTESIAN_POINT('Ctrl Pts',(57.8740741606582,-17.7220209683685,51.2694633586541));
#2623=CARTESIAN_POINT('Ctrl Pts',(57.8740741606583,-18.7864945136736,51.1007807270187));
#2624=CARTESIAN_POINT('Ctrl Pts',(57.8740741606583,-20.4196713292811,50.4516808476432));
#2625=CARTESIAN_POINT('Ctrl Pts',(57.8740741606582,-21.6797846595826,49.0661492002334));
#2626=CARTESIAN_POINT('Ctrl Pts',(57.8740741606583,-22.6517841905471,46.7445705314164));
#2627=CARTESIAN_POINT('Ctrl Pts',(57.8740741606582,-23.0108269945255,44.0387505309463));
#2628=CARTESIAN_POINT('Ctrl Pts',(57.8740741606582,-22.9578940458401,41.9269754002992));
#2629=CARTESIAN_POINT('Ctrl Pts',(57.8740741606582,-22.9057981957835,41.2086530644807));
#2630=CARTESIAN_POINT('Ctrl Pts',(56.9054158036926,-17.1175890188362,51.1244074121021));
#2631=CARTESIAN_POINT('Ctrl Pts',(56.9054158036926,-17.6866237002869,51.0489368434824));
#2632=CARTESIAN_POINT('Ctrl Pts',(56.9054158036927,-18.7381038308501,50.8806441386817));
#2633=CARTESIAN_POINT('Ctrl Pts',(56.9054158036927,-20.2899469956927,50.2606187493429));
#2634=CARTESIAN_POINT('Ctrl Pts',(56.9054158036927,-21.4843015664325,48.9508079316389));
#2635=CARTESIAN_POINT('Ctrl Pts',(56.9054158036927,-22.4335293899311,46.6958105266729));
#2636=CARTESIAN_POINT('Ctrl Pts',(56.9054158036926,-22.7876328829734,44.0257862235421));
#2637=CARTESIAN_POINT('Ctrl Pts',(56.9054158036926,-22.7347242051687,41.9363882295308));
#2638=CARTESIAN_POINT('Ctrl Pts',(56.9054158036926,-22.6831169501192,41.2248028738434));
#2639=CARTESIAN_POINT('Ctrl Pts',(56.6181896314156,-17.0392219044236,50.5335332898902));
#2640=CARTESIAN_POINT('Ctrl Pts',(56.6181896314156,-17.5919543064643,50.4602248782303));
#2641=CARTESIAN_POINT('Ctrl Pts',(56.6181896314156,-18.6094866156158,50.2919336843345));
#2642=CARTESIAN_POINT('Ctrl Pts',(56.6181896314156,-19.9424968321547,49.749699181612));
#2643=CARTESIAN_POINT('Ctrl Pts',(56.6181896314156,-20.960343635081,48.6432492760075));
#2644=CARTESIAN_POINT('Ctrl Pts',(56.6181896314156,-21.8488387330763,46.5668843895315));
#2645=CARTESIAN_POINT('Ctrl Pts',(56.6181896314156,-22.1908989647385,43.9916956640576));
#2646=CARTESIAN_POINT('Ctrl Pts',(56.6181896314156,-22.1389190953369,41.9613277687308));
#2647=CARTESIAN_POINT('Ctrl Pts',(56.6181896314156,-22.0886299869643,41.2679176457904));
#2648=CARTESIAN_POINT('Ctrl Pts',(56.6181736442213,-16.9999774720125,50.2376372405532));
#2649=CARTESIAN_POINT('Ctrl Pts',(56.6181736442213,-17.5445585268313,50.1654099348961));
#2650=CARTESIAN_POINT('Ctrl Pts',(56.6181736442213,-18.5450363459383,49.9971956031968));
#2651=CARTESIAN_POINT('Ctrl Pts',(56.6181736442213,-19.7685844487136,49.493904422604));
#2652=CARTESIAN_POINT('Ctrl Pts',(56.6181736442213,-20.6981100416586,48.489204295438));
#2653=CARTESIAN_POINT('Ctrl Pts',(56.6181736442214,-21.5561871796402,46.50222984823));
#2654=CARTESIAN_POINT('Ctrl Pts',(56.6181736442213,-21.8921327321723,43.9745858341972));
#2655=CARTESIAN_POINT('Ctrl Pts',(56.6181736442213,-21.8405547289732,41.973830798324));
#2656=CARTESIAN_POINT('Ctrl Pts',(56.6181736442213,-21.7909247107181,41.2895085231153));
#2657=CARTESIAN_POINT('',(56.6181736442213,-17.1499912781959,50.2172610306738));
#2658=CARTESIAN_POINT('',(57.0353819609965,-17.1500000599476,49.3968517751723));
#2659=CARTESIAN_POINT('Ctrl Pts',(56.6181736442213,-17.1499840472465,50.217262037498));
#2660=CARTESIAN_POINT('Ctrl Pts',(56.618171311048,-17.1500032058279,50.1732731599044));
#2661=CARTESIAN_POINT('Ctrl Pts',(56.6212228953305,-17.1500224012018,50.129369785685));
#2662=CARTESIAN_POINT('Ctrl Pts',(56.6271463571439,-17.1500372451356,50.0858125023058));
#2663=CARTESIAN_POINT('Ctrl Pts',(56.6332115081151,-17.1500524441361,50.0412133290673));
#2664=CARTESIAN_POINT('Ctrl Pts',(56.6422878813441,-17.150062913866,49.9969759001799));
#2665=CARTESIAN_POINT('Ctrl Pts',(56.6542338215383,-17.1500673466086,49.9533857272418));
#2666=CARTESIAN_POINT('Ctrl Pts',(56.6609755223862,-17.1500698482305,49.9287855784817));
#2667=CARTESIAN_POINT('Ctrl Pts',(56.6686320958241,-17.1500705022331,49.9043917713018));
#2668=CARTESIAN_POINT('Ctrl Pts',(56.6771847748605,-17.1500698498811,49.8802584871326));
#2669=CARTESIAN_POINT('Ctrl Pts',(56.6922879026331,-17.1500686978965,49.8376416564502));
#2670=CARTESIAN_POINT('Ctrl Pts',(56.7100899268355,-17.1500625613245,49.7960977151437));
#2671=CARTESIAN_POINT('Ctrl Pts',(56.7304257232293,-17.1500505789465,49.755903064599));
#2672=CARTESIAN_POINT('Ctrl Pts',(56.7505173013739,-17.1500387404682,49.7161911228205));
#2673=CARTESIAN_POINT('Ctrl Pts',(56.7730827717305,-17.1500210684331,49.6777952356117));
#2674=CARTESIAN_POINT('Ctrl Pts',(56.7980079196547,-17.1500018092014,49.6410021939523));
#2675=CARTESIAN_POINT('Ctrl Pts',(56.8213558952837,-17.1499837686235,49.6065372815436));
#2676=CARTESIAN_POINT('Ctrl Pts',(56.8467750941849,-17.1499642905174,49.5734782555144));
#2677=CARTESIAN_POINT('Ctrl Pts',(56.8742014205842,-17.1499524705361,49.5420892426593));
#2678=CARTESIAN_POINT('Ctrl Pts',(56.9034936336824,-17.1499398464098,49.5085647508953));
#2679=CARTESIAN_POINT('Ctrl Pts',(56.934889227382,-17.1499343605014,49.47715818171));
#2680=CARTESIAN_POINT('Ctrl Pts',(56.9682642728882,-17.1499494612514,49.448150109619));
#2681=CARTESIAN_POINT('Ctrl Pts',(56.9769834915822,-17.149953406317,49.4405717611669));
#2682=CARTESIAN_POINT('Ctrl Pts',(56.9858380206297,-17.1499587848582,49.4331572880387));
#2683=CARTESIAN_POINT('Ctrl Pts',(56.9948260768585,-17.1499659012595,49.425912102012));
#2684=CARTESIAN_POINT('Ctrl Pts',(57.0078460491693,-17.1499762099788,49.4154168270545));
#2685=CARTESIAN_POINT('Ctrl Pts',(57.0211461904777,-17.1499901607879,49.4052767435268));
#2686=CARTESIAN_POINT('Ctrl Pts',(57.0347099858223,-17.1500065726219,49.3954939610427));
#2687=CARTESIAN_POINT('',(56.6189035487885,-17.,50.237807097577));
#2688=CARTESIAN_POINT('Ctrl Pts',(57.03538814639,-17.1499999999997,49.3968642735726));
#2689=CARTESIAN_POINT('Ctrl Pts',(56.9904204252509,-17.1349950871205,49.4317323019518));
#2690=CARTESIAN_POINT('Ctrl Pts',(56.9448496571703,-17.1213415050968,49.4725236057591));
#2691=CARTESIAN_POINT('Ctrl Pts',(56.8147498453777,-17.0836252031835,49.6135720251987));
#2692=CARTESIAN_POINT('Ctrl Pts',(56.7451823103795,-17.0646703473624,49.7221064004491));
#2693=CARTESIAN_POINT('Ctrl Pts',(56.6485334490992,-17.0307910857937,49.9593883702037));
#2694=CARTESIAN_POINT('Ctrl Pts',(56.6221206393291,-17.0163863096898,50.0856669992656));
#2695=CARTESIAN_POINT('Ctrl Pts',(56.6189955671074,-17.0017177174059,50.2217783826396));
#2696=CARTESIAN_POINT('Ctrl Pts',(56.6189035487885,-17.0008574567801,50.2297924478132));
#2697=CARTESIAN_POINT('Ctrl Pts',(56.6189035487885,-17.,50.237807097577));
#2698=CARTESIAN_POINT('',(58.6189035487885,-17.,50.237807097577));
#2699=CARTESIAN_POINT('Origin',(57.6189035487885,-17.,50.237807097577));
#2700=CARTESIAN_POINT('Origin',(57.6189035487885,-17.,50.237807097577));
#2701=CARTESIAN_POINT('',(56.6466073920881,-17.1499031620603,50.4512837654741));
#2702=CARTESIAN_POINT('Ctrl Pts',(56.6181736442213,-16.9999774720125,50.2376372405533));
#2703=CARTESIAN_POINT('Ctrl Pts',(56.6181740497314,-17.004940043061,50.2446163905992));
#2704=CARTESIAN_POINT('Ctrl Pts',(56.6182668383978,-17.0098929123044,50.2516016942287));
#2705=CARTESIAN_POINT('Ctrl Pts',(56.6184515899688,-17.0148373029502,50.2585915972787));
#2706=CARTESIAN_POINT('Ctrl Pts',(56.6195366065838,-17.0438749234153,50.2996421870056));
#2707=CARTESIAN_POINT('Ctrl Pts',(56.6237844714869,-17.0725006077051,50.3406683752586));
#2708=CARTESIAN_POINT('Ctrl Pts',(56.6310549101252,-17.1009322593977,50.3813635864379));
#2709=CARTESIAN_POINT('Ctrl Pts',(56.6352421205432,-17.1173066920959,50.4048008810347));
#2710=CARTESIAN_POINT('Ctrl Pts',(56.6404328338326,-17.133616698542,50.4281281830798));
#2711=CARTESIAN_POINT('Ctrl Pts',(56.6466073920881,-17.1499031620603,50.4512837654741));
#2712=CARTESIAN_POINT('Ctrl Pts',(56.6466073920881,-17.1499031620601,50.4512837654741));
#2713=CARTESIAN_POINT('Ctrl Pts',(56.6362214282127,-17.1499120260523,50.4085673066142));
#2714=CARTESIAN_POINT('Ctrl Pts',(56.628577159635,-17.1499259151824,50.3652197513392));
#2715=CARTESIAN_POINT('Ctrl Pts',(56.6238417275253,-17.1499421537733,50.3214930341557));
#2716=CARTESIAN_POINT('Ctrl Pts',(56.6219795567511,-17.1499485394692,50.3042978526174));
#2717=CARTESIAN_POINT('Ctrl Pts',(56.62056775721,-17.1499553023441,50.2870439950997));
#2718=CARTESIAN_POINT('Ctrl Pts',(56.6196187380674,-17.1499623634815,50.2697468149321));
#2719=CARTESIAN_POINT('Ctrl Pts',(56.618658721881,-17.1499695064421,50.2522491985049));
#2720=CARTESIAN_POINT('Ctrl Pts',(56.6181745717269,-17.1499766632751,50.2347488876625));
#2721=CARTESIAN_POINT('Ctrl Pts',(56.6181736442213,-17.1499840472466,50.2172620374986));
#2722=CARTESIAN_POINT('',(56.6189035487885,-21.7910956063159,41.2894961290256));
#2723=CARTESIAN_POINT('Ctrl Pts',(56.6181736442213,-17.1499912781959,50.2172610306739));
#2724=CARTESIAN_POINT('Ctrl Pts',(56.6181736442213,-17.6367273439312,50.1494886908499));
#2725=CARTESIAN_POINT('Ctrl Pts',(56.6181736442213,-18.5827705834998,49.981674097399));
#2726=CARTESIAN_POINT('Ctrl Pts',(56.6181736442213,-19.7685844487136,49.493904422604));
#2727=CARTESIAN_POINT('Ctrl Pts',(56.6181736442213,-20.6981100416586,48.489204295438));
#2728=CARTESIAN_POINT('Ctrl Pts',(56.6181736442214,-21.5561871796402,46.50222984823));
#2729=CARTESIAN_POINT('Ctrl Pts',(56.6181736442213,-21.8921327321723,43.9745858341972));
#2730=CARTESIAN_POINT('Ctrl Pts',(56.6181736442213,-21.8405547289732,41.973830798324));
#2731=CARTESIAN_POINT('Ctrl Pts',(56.6181736442213,-21.7909247107181,41.2895085231153));
#2732=CARTESIAN_POINT('Origin',(57.6189035487885,-21.7910956063159,41.2894961290256));
#2733=CARTESIAN_POINT('Ctrl Pts',(58.6167627387145,-17.1602658348517,50.2165486526461));
#2734=CARTESIAN_POINT('Ctrl Pts',(58.643008473399,-16.178033900518,50.3468677070468));
#2735=CARTESIAN_POINT('Ctrl Pts',(58.2035873080419,-14.2013435692345,50.6075058158481));
#2736=CARTESIAN_POINT('Ctrl Pts',(56.2225937043736,-11.897451182557,50.9984629790502));
#2737=CARTESIAN_POINT('Ctrl Pts',(53.3892837467024,-10.8009462068176,51.3894201422522));
#2738=CARTESIAN_POINT('Ctrl Pts',(50.3736273245558,-11.1706588511001,51.7803773054543));
#2739=CARTESIAN_POINT('Ctrl Pts',(47.8891338131767,-12.9193891815025,52.1713344686563));
#2740=CARTESIAN_POINT('Ctrl Pts',(46.523451423545,-15.6333553665913,52.5622916318584));
#2741=CARTESIAN_POINT('Ctrl Pts',(46.599664491672,-18.6706201350726,52.9532487950604));
#2742=CARTESIAN_POINT('Ctrl Pts',(48.0997310899548,-21.3126898076219,53.3442059582625));
#2743=CARTESIAN_POINT('Ctrl Pts',(50.66881515933,-22.9345914086011,53.7351631214646));
#2744=CARTESIAN_POINT('Ctrl Pts',(53.6991939529023,-23.1526568531196,54.1261202846665));
#2745=CARTESIAN_POINT('Ctrl Pts',(56.47402923455,-21.9153050002011,54.5170774478686));
#2746=CARTESIAN_POINT('Ctrl Pts',(58.3369298825998,-19.5152317078047,54.9080346110706));
#2747=CARTESIAN_POINT('Ctrl Pts',(58.8472248890723,-16.5201776181574,55.2989917742727));
#2748=CARTESIAN_POINT('Ctrl Pts',(57.8842032458303,-13.6386259892673,55.6899489374747));
#2749=CARTESIAN_POINT('Ctrl Pts',(55.6756688973336,-11.5522113011612,56.0809061006768));
#2750=CARTESIAN_POINT('Ctrl Pts',(52.7440531658162,-10.7544773055472,56.4718632638789));
#2751=CARTESIAN_POINT('Ctrl Pts',(49.7828331520566,-11.4341289248563,56.8628204270809));
#2752=CARTESIAN_POINT('Ctrl Pts',(47.4924888644779,-13.430393772254,57.253777590283));
#2753=CARTESIAN_POINT('Ctrl Pts',(46.4148038926073,-16.271053097522,57.644734753485));
#2754=CARTESIAN_POINT('Ctrl Pts',(46.8047058599946,-19.2841456537754,58.035691916687));
#2755=CARTESIAN_POINT('Ctrl Pts',(48.5699630065106,-21.7569209176924,58.4266490798891));
#2756=CARTESIAN_POINT('Ctrl Pts',(51.293001714916,-23.1044410439156,58.8176062430911));
#2757=CARTESIAN_POINT('Ctrl Pts',(54.3296840336396,-23.0079485903805,59.2085634062931));
#2758=CARTESIAN_POINT('Ctrl Pts',(56.9616792526266,-21.4902689583137,59.5995205694953));
#2759=CARTESIAN_POINT('Ctrl Pts',(58.5663858627843,-18.9104110177176,59.9904777326972));
#2760=CARTESIAN_POINT('Ctrl Pts',(58.7642086619611,-15.8786431442651,60.3814348958993));
#2761=CARTESIAN_POINT('Ctrl Pts',(57.5083524385236,-13.112133530256,60.7723920591013));
#2762=CARTESIAN_POINT('Ctrl Pts',(55.095891432692,-11.2653032203185,61.1633492223034));
#2763=CARTESIAN_POINT('Ctrl Pts',(52.0974960818944,-10.77502205744,61.5543063855054));
#2764=CARTESIAN_POINT('Ctrl Pts',(49.2224402696388,-11.7572666169945,61.9452635487075));
#2765=CARTESIAN_POINT('Ctrl Pts',(47.1508217691292,-13.9796858138845,62.3362207119095));
#2766=CARTESIAN_POINT('Ctrl Pts',(46.3726843294707,-16.9165638200946,62.7271778751116));
#2767=CARTESIAN_POINT('Ctrl Pts',(47.0720972607971,-19.8731787510337,63.1181350383136));
#2768=CARTESIAN_POINT('Ctrl Pts',(49.0836136263508,-22.1501399297692,63.5090922015157));
#2769=CARTESIAN_POINT('Ctrl Pts',(51.9314069064712,-23.2088295594817,63.9000493647177));
#2770=CARTESIAN_POINT('Ctrl Pts',(54.9418283114199,-22.7988133854305,64.2910065279198));
#2771=CARTESIAN_POINT('Ctrl Pts',(57.4027591806895,-21.0170812071728,64.6819636911218));
#2772=CARTESIAN_POINT('Ctrl Pts',(58.7320634746702,-18.2851038294562,65.0729208543239));
#2773=CARTESIAN_POINT('Ctrl Pts',(58.6152927272196,-15.2491336565274,65.4638780175259));
#2774=CARTESIAN_POINT('Ctrl Pts',(57.080069193516,-12.6273329394813,65.854835180728));
#2775=CARTESIAN_POINT('Ctrl Pts',(54.4895517737208,-11.039891666206,66.24579234393));
#2776=CARTESIAN_POINT('Ctrl Pts',(51.4565303556175,-10.8623209035087,66.636749507132));
#2777=CARTESIAN_POINT('Ctrl Pts',(48.6984696589939,-12.1366252202991,67.0277066703341));
#2778=CARTESIAN_POINT('Ctrl Pts',(46.8677921271795,-14.5613664587978,67.4186638335361));
#2779=CARTESIAN_POINT('Ctrl Pts',(46.3975466451333,-17.5629692778492,67.8096209967382));
#2780=CARTESIAN_POINT('Ctrl Pts',(47.3989703241477,-20.431401064721,68.2005781599402));
#2781=CARTESIAN_POINT('Ctrl Pts',(49.6351752376468,-22.4881309646939,68.5915353231423));
#2782=CARTESIAN_POINT('Ctrl Pts',(52.5771845274374,-23.2466371494448,68.9824924863443));
#2783=CARTESIAN_POINT('Ctrl Pts',(55.529062504339,-22.5274940937726,69.3734496495464));
#2784=CARTESIAN_POINT('Ctrl Pts',(57.7925390093781,-20.5008159421237,69.7644068127484));
#2785=CARTESIAN_POINT('Ctrl Pts',(58.8321860911263,-17.6460157002987,70.1553639759505));
#2786=CARTESIAN_POINT('Ctrl Pts',(58.4020739661194,-14.6383997751071,70.5463211391525));
#2787=CARTESIAN_POINT('Ctrl Pts',(56.6039462958005,-12.189422944957,70.9372783023545));
#2788=CARTESIAN_POINT('Ctrl Pts',(53.8631519513258,-10.8783940324256,71.3282354655566));
#2789=CARTESIAN_POINT('Ctrl Pts',(50.8280296619087,-11.0154373062825,71.7191926287586));
#2790=CARTESIAN_POINT('Ctrl Pts',(48.2165396770217,-12.5681374761835,72.1101497919607));
#2791=CARTESIAN_POINT('Ctrl Pts',(46.6464360547185,-15.1691962162198,72.5011069551627));
#2792=CARTESIAN_POINT('Ctrl Pts',(46.4891218839111,-18.2033415583671,72.8920641183648));
#2793=CARTESIAN_POINT('Ctrl Pts',(47.7818243197045,-20.9528181004838,73.2830212815669));
#2794=CARTESIAN_POINT('Ctrl Pts',(50.2187210719051,-22.7672877187656,73.6739784447688));
#2795=CARTESIAN_POINT('Ctrl Pts',(53.2234261185118,-23.2174195646428,74.0649356079709));
#2796=CARTESIAN_POINT('Ctrl Pts',(56.085013860659,-22.196986288013,74.4558927711729));
#2797=CARTESIAN_POINT('Ctrl Pts',(58.1268398486099,-19.9468301996286,74.846849934375));
#2798=CARTESIAN_POINT('Ctrl Pts',(58.6189035487885,-17.9825825214271,75.1074880431764));
#2799=CARTESIAN_POINT('Ctrl Pts',(58.6189035487885,-17.,75.237807097577));
#2800=CARTESIAN_POINT('Ctrl Pts',(58.6167627387145,-17.1602658348517,49.9173493523042));
#2801=CARTESIAN_POINT('Ctrl Pts',(58.6430203769705,-16.1775884160157,50.0476684067049));
#2802=CARTESIAN_POINT('Ctrl Pts',(58.2038523387604,-14.2013635408179,50.3083065155063));
#2803=CARTESIAN_POINT('Ctrl Pts',(56.2227257314925,-11.8971076065531,50.6992636787083));
#2804=CARTESIAN_POINT('Ctrl Pts',(53.3893294286404,-10.8006864834937,51.0902208419104));
#2805=CARTESIAN_POINT('Ctrl Pts',(50.3735128366562,-11.1703590497448,51.4811780051124));
#2806=CARTESIAN_POINT('Ctrl Pts',(47.8889087174286,-12.9192014916732,51.8721351683145));
#2807=CARTESIAN_POINT('Ctrl Pts',(46.5231569839263,-15.6332855689878,52.2630923315165));
#2808=CARTESIAN_POINT('Ctrl Pts',(46.5993755176917,-18.6707023464517,52.6540494947186));
#2809=CARTESIAN_POINT('Ctrl Pts',(48.0995134617038,-21.3128963800501,53.0450066579206));
#2810=CARTESIAN_POINT('Ctrl Pts',(50.6687214804671,-22.9348772546735,53.4359638211227));
#2811=CARTESIAN_POINT('Ctrl Pts',(53.6992458585534,-23.1529526054874,53.8269209843247));
#2812=CARTESIAN_POINT('Ctrl Pts',(56.4742146877366,-21.9155415067111,54.2178781475268));
#2813=CARTESIAN_POINT('Ctrl Pts',(58.3372049022515,-19.5153526485723,54.6088353107288));
#2814=CARTESIAN_POINT('Ctrl Pts',(58.8475244706438,-16.5201545573878,54.9997924739308));
#2815=CARTESIAN_POINT('Ctrl Pts',(57.8844564990454,-13.6384643020619,55.3907496371328));
#2816=CARTESIAN_POINT('Ctrl Pts',(55.6758159259031,-11.5519492717804,55.7817068003349));
#2817=CARTESIAN_POINT('Ctrl Pts',(52.7440591848512,-10.7541769002508,56.172663963537));
#2818=CARTESIAN_POINT('Ctrl Pts',(49.7826967401103,-11.4338612127674,56.563621126739));
#2819=CARTESIAN_POINT('Ctrl Pts',(47.4922422888612,-13.4302220773222,56.9545782899411));
#2820=CARTESIAN_POINT('Ctrl Pts',(46.4145054815723,-16.2710180360713,57.3455354531431));
#2821=CARTESIAN_POINT('Ctrl Pts',(46.8044262027827,-19.2842555188512,57.7364926163451));
#2822=CARTESIAN_POINT('Ctrl Pts',(48.5697682564663,-21.7571497209455,58.1274497795472));
#2823=CARTESIAN_POINT('Ctrl Pts',(51.2929379403373,-23.1047346615051,58.5184069427492));
#2824=CARTESIAN_POINT('Ctrl Pts',(54.3297663204998,-23.0082375668037,58.9093641059513));
#2825=CARTESIAN_POINT('Ctrl Pts',(56.9618881358633,-21.4904849358282,59.3003212691533));
#2826=CARTESIAN_POINT('Ctrl Pts',(58.5666719308314,-18.9105029066094,59.6912784323554));
#2827=CARTESIAN_POINT('Ctrl Pts',(58.7645042450895,-15.878589208103,60.0822355955574));
#2828=CARTESIAN_POINT('Ctrl Pts',(57.5085876162038,-13.1119465277051,60.4731927587594));
#2829=CARTESIAN_POINT('Ctrl Pts',(55.0960105733717,-11.2650273870465,60.8641499219615));
#2830=CARTESIAN_POINT('Ctrl Pts',(52.0974710027084,-10.7747226421268,61.2551070851635));
#2831=CARTESIAN_POINT('Ctrl Pts',(49.2222769030974,-11.7570144466779,61.6460642483656));
#2832=CARTESIAN_POINT('Ctrl Pts',(47.1505587597765,-13.9795405397443,62.0370214115676));
#2833=CARTESIAN_POINT('Ctrl Pts',(46.3723838924729,-16.9165598068964,62.4279785747697));
#2834=CARTESIAN_POINT('Ctrl Pts',(47.0718304648731,-19.8733169481042,62.8189357379717));
#2835=CARTESIAN_POINT('Ctrl Pts',(49.0834435823845,-22.1503876464318,63.2098929011738));
#2836=CARTESIAN_POINT('Ctrl Pts',(51.9313738385592,-23.2091281980736,63.6008500643758));
#2837=CARTESIAN_POINT('Ctrl Pts',(54.9419400418151,-22.7990923026481,63.9918072275779));
#2838=CARTESIAN_POINT('Ctrl Pts',(57.4029892794379,-21.0172744248255,64.3827643907799));
#2839=CARTESIAN_POINT('Ctrl Pts',(58.7323575116467,-18.2851656416866,64.773721553982));
#2840=CARTESIAN_POINT('Ctrl Pts',(58.6155811476388,-15.2490494415775,65.164678717184));
#2841=CARTESIAN_POINT('Ctrl Pts',(57.0802837711922,-12.6271226185024,65.5556358803861));
#2842=CARTESIAN_POINT('Ctrl Pts',(54.4896417500622,-11.0396049908522,65.9465930435881));
#2843=CARTESIAN_POINT('Ctrl Pts',(51.4564744466051,-10.8620256872015,66.3375502067901));
#2844=CARTESIAN_POINT('Ctrl Pts',(48.6982810899941,-12.1363912967204,66.7285073699922));
#2845=CARTESIAN_POINT('Ctrl Pts',(46.8675155043528,-14.5612491630059,67.1194645331942));
#2846=CARTESIAN_POINT('Ctrl Pts',(46.3972474040464,-17.5629963559409,67.5104216963963));
#2847=CARTESIAN_POINT('Ctrl Pts',(47.3987192503709,-20.4315661121173,67.9013788595984));
#2848=CARTESIAN_POINT('Ctrl Pts',(49.6350317235223,-22.4883949375669,68.2923360228004));
#2849=CARTESIAN_POINT('Ctrl Pts',(52.5771825202072,-23.2469376083305,68.6832931860024));
#2850=CARTESIAN_POINT('Ctrl Pts',(55.5292024813889,-22.527759956937,69.0742503492045));
#2851=CARTESIAN_POINT('Ctrl Pts',(57.7927878534096,-20.5009843362785,69.4652075124065));
#2852=CARTESIAN_POINT('Ctrl Pts',(58.832484949831,-17.6460467549552,69.8561646756086));
#2853=CARTESIAN_POINT('Ctrl Pts',(58.4023521180891,-14.6382862235337,70.2471218388106));
#2854=CARTESIAN_POINT('Ctrl Pts',(56.604138000136,-12.1891914764678,70.6380790020127));
#2855=CARTESIAN_POINT('Ctrl Pts',(53.8632117382902,-10.8780997720332,71.0290361652147));
#2856=CARTESIAN_POINT('Ctrl Pts',(50.8279436516972,-11.015149059947,71.4199933284168));
#2857=CARTESIAN_POINT('Ctrl Pts',(48.2163276441712,-12.5679251643986,71.8109504916188));
#2858=CARTESIAN_POINT('Ctrl Pts',(46.6461493797905,-15.1691063153978,72.2019076548208));
#2859=CARTESIAN_POINT('Ctrl Pts',(46.4888256849871,-18.2034034662982,72.5928648180229));
#2860=CARTESIAN_POINT('Ctrl Pts',(47.781594290893,-20.9529997108187,72.983821981225));
#2861=CARTESIAN_POINT('Ctrl Pts',(50.2185986168693,-22.7675843550681,73.3747791444269));
#2862=CARTESIAN_POINT('Ctrl Pts',(53.2234648466879,-23.2176804155059,73.765736307629));
#2863=CARTESIAN_POINT('Ctrl Pts',(56.0851366634212,-22.1973332680011,74.1566934708311));
#2864=CARTESIAN_POINT('Ctrl Pts',(58.1271053182254,-19.9468173143993,74.5476506340331));
#2865=CARTESIAN_POINT('Ctrl Pts',(58.6189035487885,-17.9830281649358,74.8082887428345));
#2866=CARTESIAN_POINT('Ctrl Pts',(58.6189035487885,-17.,74.9386077972352));
#2867=CARTESIAN_POINT('Ctrl Pts',(58.330235267061,-17.1526096757125,49.3207360155538));
#2868=CARTESIAN_POINT('Ctrl Pts',(58.3552250931434,-16.2173794180463,49.4510550699545));
#2869=CARTESIAN_POINT('Ctrl Pts',(57.9367509801763,-14.3350363953506,49.7116931787559));
#2870=CARTESIAN_POINT('Ctrl Pts',(56.0504162024209,-12.1412690460258,50.1026503419579));
#2871=CARTESIAN_POINT('Ctrl Pts',(53.3524733469576,-11.0971310491503,50.49360750516));
#2872=CARTESIAN_POINT('Ctrl Pts',(50.4809080825804,-11.4491890150081,50.884564668362));
#2873=CARTESIAN_POINT('Ctrl Pts',(48.1151224405566,-13.1143598116086,51.2755218315641));
#2874=CARTESIAN_POINT('Ctrl Pts',(46.8146931916843,-15.6986545556209,51.6664789947661));
#2875=CARTESIAN_POINT('Ctrl Pts',(46.8872644702461,-18.5907973452297,52.0574361579682));
#2876=CARTESIAN_POINT('Ctrl Pts',(48.3156578215541,-21.106629044687,52.4483933211702));
#2877=CARTESIAN_POINT('Ctrl Pts',(50.7619906314754,-22.6510357393524,52.8393504843722));
#2878=CARTESIAN_POINT('Ctrl Pts',(53.6475775376757,-22.8586820898609,53.2303076475743));
#2879=CARTESIAN_POINT('Ctrl Pts',(56.2898307912776,-21.6804510319926,53.6212648107763));
#2880=CARTESIAN_POINT('Ctrl Pts',(58.0637217951495,-19.3950535957025,54.0122219739784));
#2881=CARTESIAN_POINT('Ctrl Pts',(58.5496348325434,-16.5431035947391,54.4031791371804));
#2882=CARTESIAN_POINT('Ctrl Pts',(57.6326264980959,-13.7992329061659,54.7941363003825));
#2883=CARTESIAN_POINT('Ctrl Pts',(55.5296162257536,-11.8125073984122,55.1850934635845));
#2884=CARTESIAN_POINT('Ctrl Pts',(52.7380734998907,-11.0528892445139,55.5760506267866));
#2885=CARTESIAN_POINT('Ctrl Pts',(49.9183409880472,-11.7000670149304,55.9670077899886));
#2886=CARTESIAN_POINT('Ctrl Pts',(47.7374296675502,-13.6009500518754,56.3579649531906));
#2887=CARTESIAN_POINT('Ctrl Pts',(46.7112366327447,-16.3058822813685,56.7489221163927));
#2888=CARTESIAN_POINT('Ctrl Pts',(47.0825090301861,-19.1750088583536,57.1398792795947));
#2889=CARTESIAN_POINT('Ctrl Pts',(48.7634219459444,-21.5296345779364,57.5308364427968));
#2890=CARTESIAN_POINT('Ctrl Pts',(51.3563534880287,-22.8127700060576,57.9217936059988));
#2891=CARTESIAN_POINT('Ctrl Pts',(54.247942705321,-22.7208879753013,58.3127507692009));
#2892=CARTESIAN_POINT('Ctrl Pts',(56.7541808285083,-21.2757232860857,58.7037079324029));
#2893=CARTESIAN_POINT('Ctrl Pts',(58.2822143347599,-18.8191313149124,59.094665095605));
#2894=CARTESIAN_POINT('Ctrl Pts',(58.4705851332158,-15.9322217300148,59.4856222588071));
#2895=CARTESIAN_POINT('Ctrl Pts',(57.2747338939298,-13.2978963282153,59.876579422009));
#2896=CARTESIAN_POINT('Ctrl Pts',(54.9775406088131,-11.5393078260663,60.2675365852111));
#2897=CARTESIAN_POINT('Ctrl Pts',(52.1224090028193,-11.0724523649993,60.6584937484131));
#2898=CARTESIAN_POINT('Ctrl Pts',(49.3847237551472,-12.0077651435671,61.0494509116152));
#2899=CARTESIAN_POINT('Ctrl Pts',(47.4120874732796,-14.1239968436731,61.4404080748173));
#2900=CARTESIAN_POINT('Ctrl Pts',(46.671129548173,-16.920550412317,61.8313652380193));
#2901=CARTESIAN_POINT('Ctrl Pts',(47.3371244328501,-19.7358978726952,62.2223224012214));
#2902=CARTESIAN_POINT('Ctrl Pts',(49.2525302680875,-21.904065531206,62.6132795644234));
#2903=CARTESIAN_POINT('Ctrl Pts',(51.9642555911825,-22.9121708239007,63.0042367276254));
#2904=CARTESIAN_POINT('Ctrl Pts',(54.830838644796,-22.521745279387,63.3951938908275));
#2905=CARTESIAN_POINT('Ctrl Pts',(57.1741858965679,-20.8251445111774,63.7861510540295));
#2906=CARTESIAN_POINT('Ctrl Pts',(58.4399758474222,-18.2237013906414,64.1771082172316));
#2907=CARTESIAN_POINT('Ctrl Pts',(58.3287844224443,-15.3327902927182,64.5680653804336));
#2908=CARTESIAN_POINT('Ctrl Pts',(56.8669140816383,-12.836259576758,64.9590225436357));
#2909=CARTESIAN_POINT('Ctrl Pts',(54.4001719426573,-11.3246664672051,65.3499797068377));
#2910=CARTESIAN_POINT('Ctrl Pts',(51.5120687076471,-11.1555800601186,65.7409368700398));
#2911=CARTESIAN_POINT('Ctrl Pts',(48.8857885327881,-12.3689979403138,66.1318940332418));
#2912=CARTESIAN_POINT('Ctrl Pts',(47.142581026795,-14.6778847068602,66.5228511964439));
#2913=CARTESIAN_POINT('Ctrl Pts',(46.6948039389424,-17.5360705278765,66.9138083596459));
#2914=CARTESIAN_POINT('Ctrl Pts',(47.6483794560206,-20.2674482469155,67.304765522848));
#2915=CARTESIAN_POINT('Ctrl Pts',(49.7777381892181,-22.2259073078542,67.69572268605));
#2916=CARTESIAN_POINT('Ctrl Pts',(52.5791778681548,-22.9481719616671,68.086679849252));
#2917=CARTESIAN_POINT('Ctrl Pts',(55.3900147064866,-22.2633896617156,68.4776370124541));
#2918=CARTESIAN_POINT('Ctrl Pts',(57.5453419915864,-20.3335464704585,68.8685941756561));
#2919=CARTESIAN_POINT('Ctrl Pts',(58.5353145903586,-17.6151489839351,69.2595513388582));
#2920=CARTESIAN_POINT('Ctrl Pts',(58.125753285529,-14.7512373537532,69.6505085020602));
#2921=CARTESIAN_POINT('Ctrl Pts',(56.4135403969614,-12.419272997327,70.0414656652623));
#2922=CARTESIAN_POINT('Ctrl Pts',(53.8037016011131,-11.1708851803488,70.4324228284643));
#2923=CARTESIAN_POINT('Ctrl Pts',(50.9135978412127,-11.3013806098642,70.8233799916664));
#2924=CARTESIAN_POINT('Ctrl Pts',(48.4268852822336,-12.7798923292767,71.2143371548684));
#2925=CARTESIAN_POINT('Ctrl Pts',(46.931801272795,-15.2566726002688,71.6052943180705));
#2926=CARTESIAN_POINT('Ctrl Pts',(46.7820039413394,-18.1458450190503,71.9962514812725));
#2927=CARTESIAN_POINT('Ctrl Pts',(48.012940169097,-20.7639534122315,72.3872086444746));
#2928=CARTESIAN_POINT('Ctrl Pts',(50.3334033635168,-22.4917225082625,72.7781658076765));
#2929=CARTESIAN_POINT('Ctrl Pts',(53.1945402379506,-22.9203571599847,73.1691229708786));
#2930=CARTESIAN_POINT('Ctrl Pts',(55.9194104041682,-21.9486563906518,73.5600801340807));
#2931=CARTESIAN_POINT('Ctrl Pts',(57.8636697937926,-19.8060576175284,73.9510372972827));
#2932=CARTESIAN_POINT('Ctrl Pts',(58.3322738071619,-17.9355640684967,74.2116754060841));
#2933=CARTESIAN_POINT('Ctrl Pts',(58.3322738071619,-17.,74.3419944604848));
#2934=CARTESIAN_POINT('Ctrl Pts',(57.3629302665031,-17.1267627962574,49.1017733081928));
#2935=CARTESIAN_POINT('Ctrl Pts',(57.3836892708566,-16.3498686743689,49.2320923625935));
#2936=CARTESIAN_POINT('Ctrl Pts',(57.0361245100955,-14.7863931213031,49.4927304713948));
#2937=CARTESIAN_POINT('Ctrl Pts',(55.4692526586416,-12.9641262477274,49.8836876345969));
#2938=CARTESIAN_POINT('Ctrl Pts',(53.22823777004,-12.0968409470713,50.2746447977989));
#2939=CARTESIAN_POINT('Ctrl Pts',(50.8429962491044,-12.3892668902023,50.665601961001));
#2940=CARTESIAN_POINT('Ctrl Pts',(48.8778791909101,-13.7724295894674,51.056559124203));
#2941=CARTESIAN_POINT('Ctrl Pts',(47.7976890090763,-15.9190487338459,51.4475162874051));
#2942=CARTESIAN_POINT('Ctrl Pts',(47.8579699218521,-18.3213815491006,51.8384734506071));
#2943=CARTESIAN_POINT('Ctrl Pts',(49.0444517167168,-20.4111338273766,52.2294306138092));
#2944=CARTESIAN_POINT('Ctrl Pts',(51.076475793977,-21.693981325825,52.6203877770112));
#2945=CARTESIAN_POINT('Ctrl Pts',(53.4733622037495,-21.8664607936859,53.0113449402132));
#2946=CARTESIAN_POINT('Ctrl Pts',(55.6681257696359,-20.8877739529222,53.4023021034153));
#2947=CARTESIAN_POINT('Ctrl Pts',(57.1415921405513,-18.9894294095287,53.7932592666173));
#2948=CARTESIAN_POINT('Ctrl Pts',(57.5452113735144,-16.6204831725212,54.1842164298194));
#2949=CARTESIAN_POINT('Ctrl Pts',(56.7835067669695,-14.3413120187973,54.5751735930214));
#2950=CARTESIAN_POINT('Ctrl Pts',(55.0366604743356,-12.6910566059545,54.9661307562235));
#2951=CARTESIAN_POINT('Ctrl Pts',(52.7178909811946,-12.060086717031,55.3570879194255));
#2952=CARTESIAN_POINT('Ctrl Pts',(50.3757058998908,-12.5976590270012,55.7480450826276));
#2953=CARTESIAN_POINT('Ctrl Pts',(48.5641518118953,-14.1766101762591,56.1390022458296));
#2954=CARTESIAN_POINT('Ctrl Pts',(47.711753931384,-16.4234374507423,56.5299594090317));
#2955=CARTESIAN_POINT('Ctrl Pts',(48.0201479605143,-18.8066512616149,56.9209165722337));
#2956=CARTESIAN_POINT('Ctrl Pts',(49.4163829359652,-20.7624996300655,57.3118737354358));
#2957=CARTESIAN_POINT('Ctrl Pts',(51.5701778613603,-21.8283243650465,57.7028308986378));
#2958=CARTESIAN_POINT('Ctrl Pts',(53.9720500594727,-21.7520033946092,58.0937880618398));
#2959=CARTESIAN_POINT('Ctrl Pts',(56.0538338875247,-20.5515905323791,58.4847452250419));
#2960=CARTESIAN_POINT('Ctrl Pts',(57.3230809764613,-18.5110448274855,58.8757023882439));
#2961=CARTESIAN_POINT('Ctrl Pts',(57.4795494613489,-16.1130597233218,59.266659551446));
#2962=CARTESIAN_POINT('Ctrl Pts',(56.486226541364,-13.9248813660636,59.657616714648));
#2963=CARTESIAN_POINT('Ctrl Pts',(54.5780839005581,-12.4641258735578,60.0485738778501));
#2964=CARTESIAN_POINT('Ctrl Pts',(52.2064948846027,-12.0763366447948,60.4395310410521));
#2965=CARTESIAN_POINT('Ctrl Pts',(49.9324616145104,-12.853245669751,60.8304882042542));
#2966=CARTESIAN_POINT('Ctrl Pts',(48.2939092869291,-14.6110742212096,61.2214453674562));
#2967=CARTESIAN_POINT('Ctrl Pts',(47.6784393475473,-16.9340059249544,61.6124025306583));
#2968=CARTESIAN_POINT('Ctrl Pts',(48.2316419214206,-19.2725486033772,62.0033596938603));
#2969=CARTESIAN_POINT('Ctrl Pts',(49.822656300726,-21.0735172847786,62.3943168570624));
#2970=CARTESIAN_POINT('Ctrl Pts',(52.0751261963482,-21.9108907473756,62.7852740202644));
#2971=CARTESIAN_POINT('Ctrl Pts',(54.4562272527764,-21.5865873313883,63.1762311834664));
#2972=CARTESIAN_POINT('Ctrl Pts',(56.4027072648377,-20.1773213844524,63.5671883466685));
#2973=CARTESIAN_POINT('Ctrl Pts',(57.4541241374087,-18.0164563940808,63.9581455098706));
#2974=CARTESIAN_POINT('Ctrl Pts',(57.3617639948527,-15.6151474696354,64.3491026730726));
#2975=CARTESIAN_POINT('Ctrl Pts',(56.1474747355664,-13.5414270108184,64.7400598362746));
#2976=CARTESIAN_POINT('Ctrl Pts',(54.0984978864016,-12.2858359873825,65.1310169994767));
#2977=CARTESIAN_POINT('Ctrl Pts',(51.6995212876628,-12.1453859062227,65.5219741626787));
#2978=CARTESIAN_POINT('Ctrl Pts',(49.5180256247538,-13.1533003961791,65.9129313258808));
#2979=CARTESIAN_POINT('Ctrl Pts',(48.070046216351,-15.0711561206497,66.3038884890828));
#2980=CARTESIAN_POINT('Ctrl Pts',(47.6981042642231,-17.4452820924095,66.6948456522848));
#2981=CARTESIAN_POINT('Ctrl Pts',(48.4901830662541,-19.7140760714731,67.0858028154869));
#2982=CARTESIAN_POINT('Ctrl Pts',(50.2589154680217,-21.3408522196918,67.4767599786889));
#2983=CARTESIAN_POINT('Ctrl Pts',(52.5859057745809,-21.9407947641979,67.867717141891));
#2984=CARTESIAN_POINT('Ctrl Pts',(54.9207017462093,-21.371986594498,68.258674305093));
#2985=CARTESIAN_POINT('Ctrl Pts',(56.7110046880626,-19.7689799587983,68.649631468295));
#2986=CARTESIAN_POINT('Ctrl Pts',(57.5333163950786,-17.5109678879486,69.0405886314972));
#2987=CARTESIAN_POINT('Ctrl Pts',(57.1931180318675,-15.1320858327137,69.4315457946991));
#2988=CARTESIAN_POINT('Ctrl Pts',(55.7708840250745,-13.1950609021638,69.8225029579012));
#2989=CARTESIAN_POINT('Ctrl Pts',(53.6030452317789,-12.15809898931,70.2134601211033));
#2990=CARTESIAN_POINT('Ctrl Pts',(51.2024069407833,-12.2664937492894,70.6044172843053));
#2991=CARTESIAN_POINT('Ctrl Pts',(49.1368417889046,-13.4946061863996,70.9953744475074));
#2992=CARTESIAN_POINT('Ctrl Pts',(47.8949640171512,-15.551920754989,71.3863316107094));
#2993=CARTESIAN_POINT('Ctrl Pts',(47.7705359670016,-17.9517862520598,71.7772887739114));
#2994=CARTESIAN_POINT('Ctrl Pts',(48.7930024502845,-20.1264924093384,72.1682459371135));
#2995=CARTESIAN_POINT('Ctrl Pts',(50.720472730624,-21.5616517814822,72.5592031003155));
#2996=CARTESIAN_POINT('Ctrl Pts',(53.0970522120621,-21.9176855071583,72.9501602635176));
#2997=CARTESIAN_POINT('Ctrl Pts',(55.3604335365829,-21.1105693423597,73.3411174267197));
#2998=CARTESIAN_POINT('Ctrl Pts',(56.975420845832,-19.3308053275606,73.7320745899216));
#2999=CARTESIAN_POINT('Ctrl Pts',(57.3646235473666,-17.7771714179553,73.992712698723));
#3000=CARTESIAN_POINT('Ctrl Pts',(57.3646235473666,-17.,74.1230317531237));
#3001=CARTESIAN_POINT('Ctrl Pts',(56.5845288048375,-17.1059635150217,49.7194456573622));
#3002=CARTESIAN_POINT('Ctrl Pts',(56.6018873807864,-16.4563285234116,49.8497647117628));
#3003=CARTESIAN_POINT('Ctrl Pts',(56.3114727064722,-15.1496120547916,50.1104028205642));
#3004=CARTESIAN_POINT('Ctrl Pts',(55.0016298373768,-13.6261687602616,50.5013599837662));
#3005=CARTESIAN_POINT('Ctrl Pts',(53.1282799464391,-12.9012281808381,50.8923171469683));
#3006=CARTESIAN_POINT('Ctrl Pts',(51.134332727303,-13.145653534561,51.2832743101703));
#3007=CARTESIAN_POINT('Ctrl Pts',(49.491599609735,-14.301920277547,51.6742314733724));
#3008=CARTESIAN_POINT('Ctrl Pts',(48.5886140901663,-16.0963780572031,52.0651886365744));
#3009=CARTESIAN_POINT('Ctrl Pts',(48.6390067154644,-18.1046083068019,52.4561457997765));
#3010=CARTESIAN_POINT('Ctrl Pts',(49.6308444465451,-19.8515330606131,52.8471029629785));
#3011=CARTESIAN_POINT('Ctrl Pts',(51.3295128638488,-20.9239285858085,53.2380601261806));
#3012=CARTESIAN_POINT('Ctrl Pts',(53.3331872710697,-21.0681123227409,53.6290172893826));
#3013=CARTESIAN_POINT('Ctrl Pts',(55.167897437096,-20.2499802915631,54.0199744525847));
#3014=CARTESIAN_POINT('Ctrl Pts',(56.3996399699669,-18.6630612519638,54.4109316157867));
#3015=CARTESIAN_POINT('Ctrl Pts',(56.7370450207677,-16.6827433448981,54.8018887789888));
#3016=CARTESIAN_POINT('Ctrl Pts',(56.1002989102808,-14.7774727769823,55.1928459421908));
#3017=CARTESIAN_POINT('Ctrl Pts',(54.6400247241077,-13.3979436319654,55.5838031053928));
#3018=CARTESIAN_POINT('Ctrl Pts',(52.7016519809952,-12.8704850622985,55.9747602685949));
#3019=CARTESIAN_POINT('Ctrl Pts',(50.7437050045659,-13.3198680297186,56.3657174317969));
#3020=CARTESIAN_POINT('Ctrl Pts',(49.2293384079051,-14.6397904613506,56.756674594999));
#3021=CARTESIAN_POINT('Ctrl Pts',(48.5167773612496,-16.5180231873773,57.147631758201));
#3022=CARTESIAN_POINT('Ctrl Pts',(48.7745790020052,-18.5102680842638,57.5385889214031));
#3023=CARTESIAN_POINT('Ctrl Pts',(49.9417600548431,-20.1452573217946,57.9295460846051));
#3024=CARTESIAN_POINT('Ctrl Pts',(51.7422224933087,-21.0362323067597,58.3205032478071));
#3025=CARTESIAN_POINT('Ctrl Pts',(53.750064848091,-20.9724318776226,58.7114604110092));
#3026=CARTESIAN_POINT('Ctrl Pts',(55.4903296909651,-19.9689480994622,59.1024175742113));
#3027=CARTESIAN_POINT('Ctrl Pts',(56.5513553632931,-18.263156219128,59.4933747374133));
#3028=CARTESIAN_POINT('Ctrl Pts',(56.6821550167432,-16.2585632761502,59.8843319006154));
#3029=CARTESIAN_POINT('Ctrl Pts',(55.8517878422178,-14.4293580465946,60.2752890638173));
#3030=CARTESIAN_POINT('Ctrl Pts',(54.2566781539587,-13.2082411403187,60.6662462270195));
#3031=CARTESIAN_POINT('Ctrl Pts',(52.274150991146,-12.884069171948,61.0572033902214));
#3032=CARTESIAN_POINT('Ctrl Pts',(50.3731754440476,-13.533525395032,61.4481605534236));
#3033=CARTESIAN_POINT('Ctrl Pts',(49.0034294740396,-15.0029801898505,61.8391177166255));
#3034=CARTESIAN_POINT('Ctrl Pts',(48.4889280724435,-16.9448323274048,62.2300748798276));
#3035=CARTESIAN_POINT('Ctrl Pts',(48.9513771400784,-18.8997344416325,62.6210320430297));
#3036=CARTESIAN_POINT('Ctrl Pts',(50.2813838158464,-20.405252179416,63.0119892062317));
#3037=CARTESIAN_POINT('Ctrl Pts',(52.1643334843792,-21.1052535809439,63.4029463694338));
#3038=CARTESIAN_POINT('Ctrl Pts',(54.1548122266959,-20.8341525061532,63.7939035326358));
#3039=CARTESIAN_POINT('Ctrl Pts',(55.7819699972127,-19.6560782274179,64.1848606958379));
#3040=CARTESIAN_POINT('Ctrl Pts',(56.6609007458743,-17.8497055761026,64.5758178590399));
#3041=CARTESIAN_POINT('Ctrl Pts',(56.5836923888842,-15.8423340893094,64.966775022242));
#3042=CARTESIAN_POINT('Ctrl Pts',(55.5686086522617,-14.108809810853,65.357732185444));
#3043=CARTESIAN_POINT('Ctrl Pts',(53.8557687663833,-13.0591999110719,65.748689348646));
#3044=CARTESIAN_POINT('Ctrl Pts',(51.850346984631,-12.9417908241617,66.139646511848));
#3045=CARTESIAN_POINT('Ctrl Pts',(50.0267281458869,-13.7843558051195,66.5306036750501));
#3046=CARTESIAN_POINT('Ctrl Pts',(48.8162913926872,-15.3875851347693,66.9215608382521));
#3047=CARTESIAN_POINT('Ctrl Pts',(48.5053669373851,-17.3722330628012,67.3125180014542));
#3048=CARTESIAN_POINT('Ctrl Pts',(49.1675043184158,-19.2688288307419,67.7034751646563));
#3049=CARTESIAN_POINT('Ctrl Pts',(50.6460741747913,-20.6287305163151,68.0944323278583));
#3050=CARTESIAN_POINT('Ctrl Pts',(52.5913190963785,-21.1302518109333,68.4853894910603));
#3051=CARTESIAN_POINT('Ctrl Pts',(54.5430891561779,-20.6547572603577,68.8763466542624));
#3052=CARTESIAN_POINT('Ctrl Pts',(56.0396908790909,-19.3147256772493,69.2673038174644));
#3053=CARTESIAN_POINT('Ctrl Pts',(56.7271014271941,-17.427143020902,69.6582609806665));
#3054=CARTESIAN_POINT('Ctrl Pts',(56.4427129801899,-15.4385192775656,70.0492181438685));
#3055=CARTESIAN_POINT('Ctrl Pts',(55.25379808591,-13.8192654124519,70.4401753070706));
#3056=CARTESIAN_POINT('Ctrl Pts',(53.4415956497174,-12.9524183994117,70.8311324702726));
#3057=CARTESIAN_POINT('Ctrl Pts',(51.4347848690605,-13.0430305994039,71.2220896334747));
#3058=CARTESIAN_POINT('Ctrl Pts',(49.7080778121442,-14.0696704067362,71.6130467966767));
#3059=CARTESIAN_POINT('Ctrl Pts',(48.6699319114158,-15.7894789045273,72.0040039598788));
#3060=CARTESIAN_POINT('Ctrl Pts',(48.5659154833699,-17.7956465781739,72.3949611230808));
#3061=CARTESIAN_POINT('Ctrl Pts',(49.4206471038287,-19.61358371364,72.7859182862829));
#3062=CARTESIAN_POINT('Ctrl Pts',(51.0319090823161,-20.8133168977984,73.1768754494849));
#3063=CARTESIAN_POINT('Ctrl Pts',(53.0186160188411,-21.1109153094321,73.567832612687));
#3064=CARTESIAN_POINT('Ctrl Pts',(54.9106613632555,-20.436272387398,73.958789775889));
#3065=CARTESIAN_POINT('Ctrl Pts',(56.2607295301239,-18.9483598368167,74.349746939091));
#3066=CARTESIAN_POINT('Ctrl Pts',(56.585944251621,-17.6498668651987,74.6103850478924));
#3067=CARTESIAN_POINT('Ctrl Pts',(56.585944251621,-17.,74.7407041022931));
#3068=CARTESIAN_POINT('Ctrl Pts',(56.5875334327637,-17.1060438002014,50.7124861445407));
#3069=CARTESIAN_POINT('Ctrl Pts',(56.6048933380944,-16.4563590572218,50.8428051989414));
#3070=CARTESIAN_POINT('Ctrl Pts',(56.314007219291,-15.1481902389634,51.1034433077427));
#3071=CARTESIAN_POINT('Ctrl Pts',(55.0033040235021,-13.6239537563916,51.4944004709448));
#3072=CARTESIAN_POINT('Ctrl Pts',(53.1286205132889,-12.8983806298848,51.8853576341468));
#3073=CARTESIAN_POINT('Ctrl Pts',(51.1333216249648,-13.1430309825168,52.2763147973489));
#3074=CARTESIAN_POINT('Ctrl Pts',(49.4894537168485,-14.3000624425198,52.6672719605509));
#3075=CARTESIAN_POINT('Ctrl Pts',(48.5858529064304,-16.0957627348048,53.058229123753));
#3076=CARTESIAN_POINT('Ctrl Pts',(48.6362782841291,-18.1053635807713,53.449186286955));
#3077=CARTESIAN_POINT('Ctrl Pts',(49.6287966382981,-19.8534884080997,53.840143450157));
#3078=CARTESIAN_POINT('Ctrl Pts',(51.3286289756928,-20.9266177184319,54.2311006133591));
#3079=CARTESIAN_POINT('Ctrl Pts',(53.3336769082637,-21.0709008598302,54.6220577765612));
#3080=CARTESIAN_POINT('Ctrl Pts',(55.1696445359752,-20.2522077992154,55.0130149397632));
#3081=CARTESIAN_POINT('Ctrl Pts',(56.402231363278,-18.6642011818098,55.4039721029652));
#3082=CARTESIAN_POINT('Ctrl Pts',(56.7398676601745,-16.6825258736536,55.7949292661673));
#3083=CARTESIAN_POINT('Ctrl Pts',(56.1026851208883,-14.7759494270608,56.1858864293693));
#3084=CARTESIAN_POINT('Ctrl Pts',(54.6414100340784,-13.3954747168676,56.5768435925714));
#3085=CARTESIAN_POINT('Ctrl Pts',(52.701708698725,-12.8676546237047,56.9678007557734));
#3086=CARTESIAN_POINT('Ctrl Pts',(50.7424197110664,-13.3173456033045,57.3587579189754));
#3087=CARTESIAN_POINT('Ctrl Pts',(49.2270151419221,-14.6381727336246,57.7497150821775));
#3088=CARTESIAN_POINT('Ctrl Pts',(48.5139656935336,-16.5176928320245,58.1406722453795));
#3089=CARTESIAN_POINT('Ctrl Pts',(48.7719440360339,-18.5113032479999,58.5316294085816));
#3090=CARTESIAN_POINT('Ctrl Pts',(49.9399250947533,-20.1474131350837,58.9225865717836));
#3091=CARTESIAN_POINT('Ctrl Pts',(51.7416216010786,-21.0389988096439,59.3135437349857));
#3092=CARTESIAN_POINT('Ctrl Pts',(53.7508401654488,-20.9751546505726,59.7045008981877));
#3093=CARTESIAN_POINT('Ctrl Pts',(55.4922978157049,-19.9709830674272,60.0954580613898));
#3094=CARTESIAN_POINT('Ctrl Pts',(56.5540507332295,-18.264022008069,60.4864152245918));
#3095=CARTESIAN_POINT('Ctrl Pts',(56.6849400390068,-16.2580550827007,60.8773723877939));
#3096=CARTESIAN_POINT('Ctrl Pts',(55.8540037165742,-14.4275960844986,61.2683295509959));
#3097=CARTESIAN_POINT('Ctrl Pts',(54.2578007127701,-13.2056422037469,61.659286714198));
#3098=CARTESIAN_POINT('Ctrl Pts',(52.2739146918285,-12.8812480423474,62.0502438774));
#3099=CARTESIAN_POINT('Ctrl Pts',(50.371636183478,-13.5311494138686,62.4412010406021));
#3100=CARTESIAN_POINT('Ctrl Pts',(49.0009513660834,-15.0016113982127,62.832158203804));
#3101=CARTESIAN_POINT('Ctrl Pts',(48.4860973164001,-16.9447945145355,63.2231153670061));
#3102=CARTESIAN_POINT('Ctrl Pts',(48.9488633545595,-18.9010365522097,63.6140725302082));
#3103=CARTESIAN_POINT('Ctrl Pts',(50.2797816397201,-20.4075861976786,64.0050296934103));
#3104=CARTESIAN_POINT('Ctrl Pts',(52.1640219142586,-21.1080673921761,64.3959868566123));
#3105=CARTESIAN_POINT('Ctrl Pts',(54.1558649648531,-20.8367805000576,64.7869440198143));
#3106=CARTESIAN_POINT('Ctrl Pts',(55.7841380172204,-19.6578987490017,65.1779011830163));
#3107=CARTESIAN_POINT('Ctrl Pts',(56.6636712000959,-17.8502879788808,65.5688583462184));
#3108=CARTESIAN_POINT('Ctrl Pts',(56.5864099231727,-15.8415406052356,65.9598155094205));
#3109=CARTESIAN_POINT('Ctrl Pts',(55.5706304307445,-14.1068281394938,66.3507726726225));
#3110=CARTESIAN_POINT('Ctrl Pts',(53.8566165350199,-13.0564988190924,66.7417298358246));
#3111=CARTESIAN_POINT('Ctrl Pts',(51.8498202027826,-12.9390092579546,67.1326869990265));
#3112=CARTESIAN_POINT('Ctrl Pts',(50.0249514243833,-13.7821517474598,67.5236441622287));
#3113=CARTESIAN_POINT('Ctrl Pts',(48.8136850171062,-15.3864799578778,67.9146013254307));
#3114=CARTESIAN_POINT('Ctrl Pts',(48.5025474487642,-17.3724881979037,68.3055584886327));
#3115=CARTESIAN_POINT('Ctrl Pts',(49.1651386702972,-19.2703839245662,68.6965156518348));
#3116=CARTESIAN_POINT('Ctrl Pts',(50.6447219634242,-20.6312177112838,69.0874728150368));
#3117=CARTESIAN_POINT('Ctrl Pts',(52.5913001901039,-21.1330827546075,69.4784299782389));
#3118=CARTESIAN_POINT('Ctrl Pts',(54.5444080247444,-20.657262297519,69.8693871414409));
#3119=CARTESIAN_POINT('Ctrl Pts',(56.0420355481367,-19.3163122216428,70.2603443046429));
#3120=CARTESIAN_POINT('Ctrl Pts',(56.72991725061,-17.427435809996,70.651301467845));
#3121=CARTESIAN_POINT('Ctrl Pts',(56.4453338975223,-15.4374489730838,71.042258631047));
#3122=CARTESIAN_POINT('Ctrl Pts',(55.255604060317,-13.8170853662882,71.4332157942491));
#3123=CARTESIAN_POINT('Ctrl Pts',(53.4421595967455,-12.9496439359626,71.8241729574512));
#3124=CARTESIAN_POINT('Ctrl Pts',(51.4339731256248,-13.0403188167553,72.2151301206532));
#3125=CARTESIAN_POINT('Ctrl Pts',(49.7060829637914,-14.067661057971,72.6060872838552));
#3126=CARTESIAN_POINT('Ctrl Pts',(48.6672246276916,-15.7886510209866,72.9970444470573));
#3127=CARTESIAN_POINT('Ctrl Pts',(48.5631388489693,-17.7961879271213,73.3880016102593));
#3128=CARTESIAN_POINT('Ctrl Pts',(49.4184523520201,-19.6153835669027,73.7789587734614));
#3129=CARTESIAN_POINT('Ctrl Pts',(51.0308282898254,-20.8159115065848,74.1699159366634));
#3130=CARTESIAN_POINT('Ctrl Pts',(53.0188804033209,-21.1137709412463,74.5608730998655));
#3131=CARTESIAN_POINT('Ctrl Pts',(54.912275787121,-20.4385313200904,74.9518302630675));
#3132=CARTESIAN_POINT('Ctrl Pts',(56.2632251605407,-18.9498488446407,75.3427874262696));
#3133=CARTESIAN_POINT('Ctrl Pts',(56.5889499519861,-17.6499166343259,75.6034255350709));
#3134=CARTESIAN_POINT('Ctrl Pts',(56.5889499519861,-17.,75.7337445894716));
#3135=CARTESIAN_POINT('Ctrl Pts',(57.3618632631907,-17.1267342853886,51.3345782519786));
#3136=CARTESIAN_POINT('Ctrl Pts',(57.3826228523727,-16.3498182766226,51.4648973063793));
#3137=CARTESIAN_POINT('Ctrl Pts',(57.0352479861203,-14.7868998097433,51.7255354151806));
#3138=CARTESIAN_POINT('Ctrl Pts',(55.4686698444437,-12.9648823336634,52.1164925783827));
#3139=CARTESIAN_POINT('Ctrl Pts',(53.2281208840586,-12.0978291083762,52.5074497415848));
#3140=CARTESIAN_POINT('Ctrl Pts',(50.8433451463302,-12.3901715913768,52.8984069047868));
#3141=CARTESIAN_POINT('Ctrl Pts',(48.8786212540224,-13.7730726787602,53.2893640679889));
#3142=CARTESIAN_POINT('Ctrl Pts',(47.7986434171988,-15.9192610497727,53.6803212311909));
#3143=CARTESIAN_POINT('Ctrl Pts',(47.8589131842379,-18.3211206357986,54.0712783943929));
#3144=CARTESIAN_POINT('Ctrl Pts',(49.0451596110562,-20.4104577860508,54.462235557595));
#3145=CARTESIAN_POINT('Ctrl Pts',(51.0767813625441,-21.6930517414687,54.853192720797));
#3146=CARTESIAN_POINT('Ctrl Pts',(53.4731929325189,-21.8654967884011,55.2441498839991));
#3147=CARTESIAN_POINT('Ctrl Pts',(55.6675218063666,-20.8870039199405,55.6351070472011));
#3148=CARTESIAN_POINT('Ctrl Pts',(57.1406963040962,-18.9890353360354,56.0260642104031));
#3149=CARTESIAN_POINT('Ctrl Pts',(57.5442355978115,-16.6205583533319,56.4170213736052));
#3150=CARTESIAN_POINT('Ctrl Pts',(56.782681862343,-14.3418386345305,56.8079785368072));
#3151=CARTESIAN_POINT('Ctrl Pts',(55.0361815778019,-12.6919101013593,57.1989357000093));
#3152=CARTESIAN_POINT('Ctrl Pts',(52.7178713740276,-12.0610651892422,57.5898928632113));
#3153=CARTESIAN_POINT('Ctrl Pts',(50.3761502212309,-12.598531020774,57.9808500264134));
#3154=CARTESIAN_POINT('Ctrl Pts',(48.5649549565342,-14.1771694188471,58.3718071896154));
#3155=CARTESIAN_POINT('Ctrl Pts',(47.7127259147526,-16.4235516534108,58.7627643528175));
#3156=CARTESIAN_POINT('Ctrl Pts',(48.021058858721,-18.8062934092461,59.1537215160195));
#3157=CARTESIAN_POINT('Ctrl Pts',(49.4170172750347,-20.7617543732099,59.5446786792216));
#3158=CARTESIAN_POINT('Ctrl Pts',(51.5703855876311,-21.8273679950004,59.9356358424236));
#3159=CARTESIAN_POINT('Ctrl Pts',(53.9717820350656,-21.7510621418458,60.3265930056256));
#3160=CARTESIAN_POINT('Ctrl Pts',(56.0531535139181,-20.550887051311,60.7175501688278));
#3161=CARTESIAN_POINT('Ctrl Pts',(57.3221491968199,-18.5107455273791,61.1085073320297));
#3162=CARTESIAN_POINT('Ctrl Pts',(57.4785866892221,-16.1132354039597,61.4994644952318));
#3163=CARTESIAN_POINT('Ctrl Pts',(56.4854605216108,-13.9254904699895,61.8904216584338));
#3164=CARTESIAN_POINT('Ctrl Pts',(54.5776958360358,-12.4650243165339,62.2813788216359));
#3165=CARTESIAN_POINT('Ctrl Pts',(52.2065765724224,-12.0773118990975,62.6723359848379));
#3166=CARTESIAN_POINT('Ctrl Pts',(49.9329937313239,-12.8540670378484,63.06329314804));
#3167=CARTESIAN_POINT('Ctrl Pts',(48.2947659598895,-14.6115474075297,63.454250311242));
#3168=CARTESIAN_POINT('Ctrl Pts',(47.6794179296765,-16.9340189967265,63.8452074744441));
#3169=CARTESIAN_POINT('Ctrl Pts',(48.2325109279855,-19.2720984684587,64.2361646376461));
#3170=CARTESIAN_POINT('Ctrl Pts',(49.82321016722,-21.0727104231042,64.6271218008482));
#3171=CARTESIAN_POINT('Ctrl Pts',(52.0752339050124,-21.9099180230063,65.0180789640502));
#3172=CARTESIAN_POINT('Ctrl Pts',(54.4558633250017,-21.5856788433975,65.4090361272523));
#3173=CARTESIAN_POINT('Ctrl Pts',(56.4019577881599,-20.1766920367232,65.7999932904543));
#3174=CARTESIAN_POINT('Ctrl Pts',(57.4531664014012,-18.0162550595463,66.1909504536564));
#3175=CARTESIAN_POINT('Ctrl Pts',(57.3608245530749,-15.6154217742106,66.5819076168584));
#3176=CARTESIAN_POINT('Ctrl Pts',(56.1467758140548,-13.5421120674427,66.9728647800605));
#3177=CARTESIAN_POINT('Ctrl Pts',(54.0982048158494,-12.2867697451128,67.3638219432625));
#3178=CARTESIAN_POINT('Ctrl Pts',(51.6997033942426,-12.1463474836051,67.7547791064645));
#3179=CARTESIAN_POINT('Ctrl Pts',(49.5186398309548,-13.1540623309393,68.1457362696666));
#3180=CARTESIAN_POINT('Ctrl Pts',(48.0709472309629,-15.0715381763131,68.5366934328686));
#3181=CARTESIAN_POINT('Ctrl Pts',(47.6990789512508,-17.4451938931097,68.9276505960707));
#3182=CARTESIAN_POINT('Ctrl Pts',(48.491000862243,-19.7135384811981,69.3186077592727));
#3183=CARTESIAN_POINT('Ctrl Pts',(50.2593829226289,-21.3399924053029,69.7095649224748));
#3184=CARTESIAN_POINT('Ctrl Pts',(52.585912310354,-21.9398161173807,70.1005220856768));
#3185=CARTESIAN_POINT('Ctrl Pts',(54.9202458182389,-21.3711206118296,70.4914792488789));
#3186=CARTESIAN_POINT('Ctrl Pts',(56.7101941441817,-19.7684314969577,70.8824364120809));
#3187=CARTESIAN_POINT('Ctrl Pts',(57.5323429756866,-17.5108666700446,71.273393575283));
#3188=CARTESIAN_POINT('Ctrl Pts',(57.1922119889622,-15.1324558369381,71.664350738485));
#3189=CARTESIAN_POINT('Ctrl Pts',(55.7702597089705,-13.1958145279503,72.055307901687));
#3190=CARTESIAN_POINT('Ctrl Pts',(53.602850271426,-12.159058129237,72.4462650648891));
#3191=CARTESIAN_POINT('Ctrl Pts',(51.2026875702207,-12.267431164002,72.8372222280911));
#3192=CARTESIAN_POINT('Ctrl Pts',(49.1375313729449,-13.495300895059,73.2281793912932));
#3193=CARTESIAN_POINT('Ctrl Pts',(47.8958999737314,-15.5522067706523,73.6191365544952));
#3194=CARTESIAN_POINT('Ctrl Pts',(47.7714957057545,-17.9515995050567,74.0100937176972));
#3195=CARTESIAN_POINT('Ctrl Pts',(48.7937614261677,-20.1258693707283,74.4010508808993));
#3196=CARTESIAN_POINT('Ctrl Pts',(50.7208456688109,-21.5607567224907,74.7920080441013));
#3197=CARTESIAN_POINT('Ctrl Pts',(53.0969617625352,-21.9166945762927,75.1829652073034));
#3198=CARTESIAN_POINT('Ctrl Pts',(55.3598711261245,-21.1097979586625,75.5739223705055));
#3199=CARTESIAN_POINT('Ctrl Pts',(56.974558168743,-19.3302754071,75.9648795337075));
#3200=CARTESIAN_POINT('Ctrl Pts',(57.3635561632098,-17.7771933126448,76.2255176425089));
#3201=CARTESIAN_POINT('Ctrl Pts',(57.3635561632098,-17.,76.3558366969096));
#3202=CARTESIAN_POINT('Ctrl Pts',(58.3303540870803,-17.1526128506436,51.1101091552529));
#3203=CARTESIAN_POINT('Ctrl Pts',(58.355341642541,-16.2174675697245,51.2404282096536));
#3204=CARTESIAN_POINT('Ctrl Pts',(57.9367994837362,-14.3349762708849,51.5010663184549));
#3205=CARTESIAN_POINT('Ctrl Pts',(56.0504566417972,-12.1412485071656,51.8920234816569));
#3206=CARTESIAN_POINT('Ctrl Pts',(53.3524778992612,-11.097069130456,52.282980644859));
#3207=CARTESIAN_POINT('Ctrl Pts',(50.480890442206,-11.4491438159843,52.6739378080611));
#3208=CARTESIAN_POINT('Ctrl Pts',(48.1150815112142,-13.1143229732784,53.0648949712631));
#3209=CARTESIAN_POINT('Ctrl Pts',(46.8146414639397,-15.6986438445251,53.4558521344651));
#3210=CARTESIAN_POINT('Ctrl Pts',(46.8872129710008,-18.5908111680355,53.8468092976672));
#3211=CARTESIAN_POINT('Ctrl Pts',(48.3156193136198,-21.1066660539386,54.2377664608693));
#3212=CARTESIAN_POINT('Ctrl Pts',(50.7619739606184,-22.6510862949705,54.6287236240713));
#3213=CARTESIAN_POINT('Ctrl Pts',(53.6475867703978,-22.8587346431059,55.0196807872733));
#3214=CARTESIAN_POINT('Ctrl Pts',(56.2898636869932,-21.680492961833,55.4106379504754));
#3215=CARTESIAN_POINT('Ctrl Pts',(58.0637705985691,-19.3950750712552,55.8015951136774));
#3216=CARTESIAN_POINT('Ctrl Pts',(58.5496879870503,-16.5430994954114,56.1925522768795));
#3217=CARTESIAN_POINT('Ctrl Pts',(57.6326714355344,-13.7992042203998,56.5835094400815));
#3218=CARTESIAN_POINT('Ctrl Pts',(55.5296423135302,-11.8124609031937,56.9744666032836));
#3219=CARTESIAN_POINT('Ctrl Pts',(52.7380745681098,-11.0528359423474,57.3654237664856));
#3220=CARTESIAN_POINT('Ctrl Pts',(49.9183167834665,-11.7000195126523,57.7563809296876));
#3221=CARTESIAN_POINT('Ctrl Pts',(47.7373859160472,-13.6009195870612,58.1473380928897));
#3222=CARTESIAN_POINT('Ctrl Pts',(46.7111836836696,-16.305876060109,58.5382952560918));
#3223=CARTESIAN_POINT('Ctrl Pts',(47.0824594087586,-19.1750283524781,58.9292524192938));
#3224=CARTESIAN_POINT('Ctrl Pts',(48.7633873901451,-21.5296751760025,59.3202095824958));
#3225=CARTESIAN_POINT('Ctrl Pts',(51.3563421720835,-22.812822104585,59.7111667456979));
#3226=CARTESIAN_POINT('Ctrl Pts',(54.2479573060245,-22.7209392503051,60.1021239088999));
#3227=CARTESIAN_POINT('Ctrl Pts',(56.7542178920496,-21.275761608413,60.493081072102));
#3228=CARTESIAN_POINT('Ctrl Pts',(58.2822650937144,-18.8191476193684,60.884038235304));
#3229=CARTESIAN_POINT('Ctrl Pts',(58.4706375804947,-15.9322121597635,61.2749953985061));
#3230=CARTESIAN_POINT('Ctrl Pts',(57.2747756230685,-13.2978631471098,61.6659525617081));
#3231=CARTESIAN_POINT('Ctrl Pts',(54.9775617487357,-11.5392588831358,62.0569097249102));
#3232=CARTESIAN_POINT('Ctrl Pts',(52.1224045528526,-11.0723992377504,62.4478668881122));
#3233=CARTESIAN_POINT('Ctrl Pts',(49.3846947679361,-12.007720399312,62.8388240513143));
#3234=CARTESIAN_POINT('Ctrl Pts',(47.4120408057822,-14.1239710667169,63.2297812145162));
#3235=CARTESIAN_POINT('Ctrl Pts',(46.6710762396398,-16.9205497002286,63.6207383777184));
#3236=CARTESIAN_POINT('Ctrl Pts',(47.3370770934763,-19.7359223939198,64.0116955409204));
#3237=CARTESIAN_POINT('Ctrl Pts',(49.2525000960564,-21.9041094852197,64.4026527041224));
#3238=CARTESIAN_POINT('Ctrl Pts',(51.9642497237231,-22.9122238133307,64.7936098673245));
#3239=CARTESIAN_POINT('Ctrl Pts',(54.8308584698625,-22.5217947695224,65.1845670305265));
#3240=CARTESIAN_POINT('Ctrl Pts',(57.1742267245179,-20.8251787950697,65.5755241937285));
#3241=CARTESIAN_POINT('Ctrl Pts',(58.4400280203571,-18.2237123583959,65.9664813569306));
#3242=CARTESIAN_POINT('Ctrl Pts',(58.3288355987958,-15.3327753499006,66.3574385201327));
#3243=CARTESIAN_POINT('Ctrl Pts',(56.8669521555819,-12.8362222581074,66.7483956833347));
#3244=CARTESIAN_POINT('Ctrl Pts',(54.4001879077564,-11.3246156004952,67.1393528465368));
#3245=CARTESIAN_POINT('Ctrl Pts',(51.5120587873418,-11.1555276779201,67.5303100097388));
#3246=CARTESIAN_POINT('Ctrl Pts',(48.8857550737321,-12.3689564337142,67.9212671729409));
#3247=CARTESIAN_POINT('Ctrl Pts',(47.1425319437795,-14.6778638942547,68.3122243361429));
#3248=CARTESIAN_POINT('Ctrl Pts',(46.6947508425837,-17.536075332595,68.7031814993449));
#3249=CARTESIAN_POINT('Ctrl Pts',(47.6483349063834,-20.2674775322146,69.094138662547));
#3250=CARTESIAN_POINT('Ctrl Pts',(49.7777127244415,-22.2259541466555,69.485095825749));
#3251=CARTESIAN_POINT('Ctrl Pts',(52.5791775122401,-22.9482252733484,69.8760529889511));
#3252=CARTESIAN_POINT('Ctrl Pts',(55.3900395430226,-22.2634368371744,70.2670101521531));
#3253=CARTESIAN_POINT('Ctrl Pts',(57.5453861467663,-20.3335763463122,70.6579673153551));
#3254=CARTESIAN_POINT('Ctrl Pts',(58.5353676164029,-17.6151545016087,71.0489244785573));
#3255=CARTESIAN_POINT('Ctrl Pts',(58.1258026451683,-14.7512171894498,71.4398816417592));
#3256=CARTESIAN_POINT('Ctrl Pts',(56.4135744009266,-12.4192319611238,71.8308388049613));
#3257=CARTESIAN_POINT('Ctrl Pts',(53.8037122342891,-11.1708328924698,72.2217959681633));
#3258=CARTESIAN_POINT('Ctrl Pts',(50.9135825266937,-11.3013296269896,72.6127531313654));
#3259=CARTESIAN_POINT('Ctrl Pts',(48.4268477765921,-12.7798543046457,73.0037102945674));
#3260=CARTESIAN_POINT('Ctrl Pts',(46.9317501611453,-15.2566574068001,73.3946674577695));
#3261=CARTESIAN_POINT('Ctrl Pts',(46.7819519459475,-18.1458543446259,73.7856246209715));
#3262=CARTESIAN_POINT('Ctrl Pts',(48.0128982703705,-20.7639891441552,74.1765817841736));
#3263=CARTESIAN_POINT('Ctrl Pts',(50.3333845221266,-22.4917672199676,74.5675389473756));
#3264=CARTESIAN_POINT('Ctrl Pts',(53.1945431347214,-22.9204191781828,74.9584961105777));
#3265=CARTESIAN_POINT('Ctrl Pts',(55.9194502805027,-21.9486780023587,75.3494532737797));
#3266=CARTESIAN_POINT('Ctrl Pts',(57.8637166740634,-19.8061190161188,75.7404104369818));
#3267=CARTESIAN_POINT('Ctrl Pts',(58.3323926695916,-17.9354790614188,76.0010485457831));
#3268=CARTESIAN_POINT('Ctrl Pts',(58.3323926695916,-17.,76.1313676001838));
#3269=CARTESIAN_POINT('Ctrl Pts',(58.6167627387145,-17.1602658348517,50.515747952988));
#3270=CARTESIAN_POINT('Ctrl Pts',(58.643021929101,-16.1775303283992,50.6460670073887));
#3271=CARTESIAN_POINT('Ctrl Pts',(58.2038868966466,-14.2013661449526,50.90670511619));
#3272=CARTESIAN_POINT('Ctrl Pts',(56.2227429467729,-11.8970628069899,51.2976622793921));
#3273=CARTESIAN_POINT('Ctrl Pts',(53.3893353851998,-10.8006526176493,51.6886194425942));
#3274=CARTESIAN_POINT('Ctrl Pts',(50.3734979083497,-11.1703199580457,52.0795766057962));
#3275=CARTESIAN_POINT('Ctrl Pts',(47.8888793667432,-12.9191770184205,52.4705337689982));
#3276=CARTESIAN_POINT('Ctrl Pts',(46.5231185913547,-15.6332764679385,52.8614909322003));
#3277=CARTESIAN_POINT('Ctrl Pts',(46.5993378377957,-18.670713066158,53.2524480954023));
#3278=CARTESIAN_POINT('Ctrl Pts',(48.0994850847202,-21.3129233154427,53.6434052586044));
#3279=CARTESIAN_POINT('Ctrl Pts',(50.6687092654925,-22.9349145267153,54.0343624218064));
#3280=CARTESIAN_POINT('Ctrl Pts',(53.6992526266351,-23.1529911692309,54.4253195850084));
#3281=CARTESIAN_POINT('Ctrl Pts',(56.474238869349,-21.9155723452686,54.8162767482105));
#3282=CARTESIAN_POINT('Ctrl Pts',(58.3372407626147,-19.5153684182812,55.2072339114125));
#3283=CARTESIAN_POINT('Ctrl Pts',(58.8475635336849,-16.5201515504479,55.5981910746146));
#3284=CARTESIAN_POINT('Ctrl Pts',(57.8844895212394,-13.6384432193433,55.9891482378167));
#3285=CARTESIAN_POINT('Ctrl Pts',(55.6758350972527,-11.5519151052446,56.3801054010187));
#3286=CARTESIAN_POINT('Ctrl Pts',(52.7440599696852,-10.7541377298025,56.7710625642207));
#3287=CARTESIAN_POINT('Ctrl Pts',(49.7826789530834,-11.433826305252,57.1620197274228));
#3288=CARTESIAN_POINT('Ctrl Pts',(47.4922101373727,-13.4301996896761,57.5529768906249));
#3289=CARTESIAN_POINT('Ctrl Pts',(46.4144665711598,-16.2710134643385,57.9439340538269));
#3290=CARTESIAN_POINT('Ctrl Pts',(46.8043897377188,-19.2842698443785,58.3348912170289));
#3291=CARTESIAN_POINT('Ctrl Pts',(48.569742862618,-21.7571795550599,58.7258483802309));
#3292=CARTESIAN_POINT('Ctrl Pts',(51.2929296246423,-23.1047729468906,59.116805543433));
#3293=CARTESIAN_POINT('Ctrl Pts',(54.3297770500483,-23.0082752470182,59.507762706635));
#3294=CARTESIAN_POINT('Ctrl Pts',(56.9619153725668,-21.4905130975688,59.8987198698371));
#3295=CARTESIAN_POINT('Ctrl Pts',(58.566709231817,-18.910514888186,60.2896770330391));
#3296=CARTESIAN_POINT('Ctrl Pts',(58.7645427867655,-15.8785821752588,60.6806341962412));
#3297=CARTESIAN_POINT('Ctrl Pts',(57.5086182814925,-13.111922144068,61.0715913594432));
#3298=CARTESIAN_POINT('Ctrl Pts',(55.0960261083635,-11.2649914205938,61.4625485226453));
#3299=CARTESIAN_POINT('Ctrl Pts',(52.0974677325831,-10.7746836007645,61.8535056858473));
#3300=CARTESIAN_POINT('Ctrl Pts',(49.2222556014069,-11.7569815656853,62.2444628490494));
#3301=CARTESIAN_POINT('Ctrl Pts',(47.1505244654603,-13.9795215971582,62.6354200122514));
#3302=CARTESIAN_POINT('Ctrl Pts',(46.3723447178911,-16.9165592836075,63.0263771754535));
#3303=CARTESIAN_POINT('Ctrl Pts',(47.0717956768182,-19.873334967897,63.4173343386555));
#3304=CARTESIAN_POINT('Ctrl Pts',(49.0834214100111,-22.1504199467036,63.8082915018576));
#3305=CARTESIAN_POINT('Ctrl Pts',(51.9313695267679,-23.2091671381576,64.1992486650596));
#3306=CARTESIAN_POINT('Ctrl Pts',(54.9419546105651,-22.7991286712227,64.5902058282616));
#3307=CARTESIAN_POINT('Ctrl Pts',(57.4030192824745,-21.0172996188621,64.9811629914637));
#3308=CARTESIAN_POINT('Ctrl Pts',(58.7323958517169,-18.2851737015071,65.3721201546658));
#3309=CARTESIAN_POINT('Ctrl Pts',(58.6156187553549,-15.2490384606216,65.7630773178678));
#3310=CARTESIAN_POINT('Ctrl Pts',(57.0803117504052,-12.6270951943288,66.1540344810699));
#3311=CARTESIAN_POINT('Ctrl Pts',(54.4896534822575,-11.0395676106787,66.5449916442719));
#3312=CARTESIAN_POINT('Ctrl Pts',(51.456467156517,-10.861987193356,66.9359488074739));
#3313=CARTESIAN_POINT('Ctrl Pts',(48.6982565021046,-12.1363607949564,67.326905970676));
#3314=CARTESIAN_POINT('Ctrl Pts',(46.8674794349484,-14.5612338685727,67.717863133878));
#3315=CARTESIAN_POINT('Ctrl Pts',(46.3972083854018,-17.5629998867075,68.1088202970801));
#3316=CARTESIAN_POINT('Ctrl Pts',(47.3986865123584,-20.4315876329779,68.4997774602821));
#3317=CARTESIAN_POINT('Ctrl Pts',(49.6350130104282,-22.4884293575185,68.8907346234842));
#3318=CARTESIAN_POINT('Ctrl Pts',(52.5771822584804,-23.2469767857663,69.2816917866862));
#3319=CARTESIAN_POINT('Ctrl Pts',(55.5292207332768,-22.5277946233674,69.6726489498883));
#3320=CARTESIAN_POINT('Ctrl Pts',(57.7928203006812,-20.5010062935296,70.0636061130903));
#3321=CARTESIAN_POINT('Ctrl Pts',(58.8325239186161,-17.6460508042341,70.4545632762924));
#3322=CARTESIAN_POINT('Ctrl Pts',(58.4023883868815,-14.6382714173167,70.8455204394944));
#3323=CARTESIAN_POINT('Ctrl Pts',(56.6041629968483,-12.1891612948279,71.2364776026964));
#3324=CARTESIAN_POINT('Ctrl Pts',(53.8632195340322,-10.8780614028313,71.6274347658985));
#3325=CARTESIAN_POINT('Ctrl Pts',(50.8279324366534,-11.01511147493,72.0183919291005));
#3326=CARTESIAN_POINT('Ctrl Pts',(48.2162999967831,-12.5678974806397,72.4093490923026));
#3327=CARTESIAN_POINT('Ctrl Pts',(46.6461119996725,-15.1690945930496,72.8003062555046));
#3328=CARTESIAN_POINT('Ctrl Pts',(46.4887870630162,-18.2034115385973,73.1912634187066));
#3329=CARTESIAN_POINT('Ctrl Pts',(47.7815642969756,-20.953023391354,73.5822205819087));
#3330=CARTESIAN_POINT('Ctrl Pts',(50.2185826497119,-22.7676230340697,73.9731777451107));
#3331=CARTESIAN_POINT('Ctrl Pts',(53.2234698965323,-23.2177144283724,74.3641349083128));
#3332=CARTESIAN_POINT('Ctrl Pts',(56.0851526759193,-22.1973785114167,74.7550920715148));
#3333=CARTESIAN_POINT('Ctrl Pts',(58.1271399333403,-19.9468156342685,75.1460492347169));
#3334=CARTESIAN_POINT('Ctrl Pts',(58.6189035487885,-17.9830862732854,75.4066873435182));
#3335=CARTESIAN_POINT('Ctrl Pts',(58.6189035487885,-17.,75.5370063979189));
#3336=CARTESIAN_POINT('Ctrl Pts',(58.6167627387145,-17.1602658348517,50.2165486526461));
#3337=CARTESIAN_POINT('Ctrl Pts',(58.643008473399,-16.178033900518,50.3468677070468));
#3338=CARTESIAN_POINT('Ctrl Pts',(58.2035873080419,-14.2013435692345,50.6075058158482));
#3339=CARTESIAN_POINT('Ctrl Pts',(56.2225937043736,-11.897451182557,50.9984629790502));
#3340=CARTESIAN_POINT('Ctrl Pts',(53.3892837467024,-10.8009462068176,51.3894201422522));
#3341=CARTESIAN_POINT('Ctrl Pts',(50.3736273245558,-11.1706588511001,51.7803773054543));
#3342=CARTESIAN_POINT('Ctrl Pts',(47.8891338131767,-12.9193891815025,52.1713344686563));
#3343=CARTESIAN_POINT('Ctrl Pts',(46.523451423545,-15.6333553665913,52.5622916318584));
#3344=CARTESIAN_POINT('Ctrl Pts',(46.599664491672,-18.6706201350726,52.9532487950604));
#3345=CARTESIAN_POINT('Ctrl Pts',(48.0997310899548,-21.3126898076219,53.3442059582625));
#3346=CARTESIAN_POINT('Ctrl Pts',(50.66881515933,-22.9345914086011,53.7351631214646));
#3347=CARTESIAN_POINT('Ctrl Pts',(53.6991939529023,-23.1526568531196,54.1261202846665));
#3348=CARTESIAN_POINT('Ctrl Pts',(56.47402923455,-21.9153050002011,54.5170774478686));
#3349=CARTESIAN_POINT('Ctrl Pts',(58.3369298825998,-19.5152317078047,54.9080346110706));
#3350=CARTESIAN_POINT('Ctrl Pts',(58.8472248890723,-16.5201776181574,55.2989917742727));
#3351=CARTESIAN_POINT('Ctrl Pts',(57.8842032458303,-13.6386259892673,55.6899489374747));
#3352=CARTESIAN_POINT('Ctrl Pts',(55.6756688973336,-11.5522113011612,56.0809061006768));
#3353=CARTESIAN_POINT('Ctrl Pts',(52.7440531658162,-10.7544773055472,56.4718632638789));
#3354=CARTESIAN_POINT('Ctrl Pts',(49.7828331520566,-11.4341289248563,56.8628204270809));
#3355=CARTESIAN_POINT('Ctrl Pts',(47.4924888644779,-13.430393772254,57.253777590283));
#3356=CARTESIAN_POINT('Ctrl Pts',(46.4148038926073,-16.271053097522,57.644734753485));
#3357=CARTESIAN_POINT('Ctrl Pts',(46.8047058599946,-19.2841456537754,58.035691916687));
#3358=CARTESIAN_POINT('Ctrl Pts',(48.5699630065106,-21.7569209176924,58.4266490798891));
#3359=CARTESIAN_POINT('Ctrl Pts',(51.293001714916,-23.1044410439156,58.8176062430911));
#3360=CARTESIAN_POINT('Ctrl Pts',(54.3296840336396,-23.0079485903805,59.2085634062931));
#3361=CARTESIAN_POINT('Ctrl Pts',(56.9616792526266,-21.4902689583137,59.5995205694953));
#3362=CARTESIAN_POINT('Ctrl Pts',(58.5663858627843,-18.9104110177176,59.9904777326972));
#3363=CARTESIAN_POINT('Ctrl Pts',(58.7642086619611,-15.8786431442651,60.3814348958993));
#3364=CARTESIAN_POINT('Ctrl Pts',(57.5083524385236,-13.112133530256,60.7723920591013));
#3365=CARTESIAN_POINT('Ctrl Pts',(55.095891432692,-11.2653032203185,61.1633492223034));
#3366=CARTESIAN_POINT('Ctrl Pts',(52.0974960818944,-10.77502205744,61.5543063855054));
#3367=CARTESIAN_POINT('Ctrl Pts',(49.2224402696388,-11.7572666169945,61.9452635487075));
#3368=CARTESIAN_POINT('Ctrl Pts',(47.1508217691292,-13.9796858138845,62.3362207119095));
#3369=CARTESIAN_POINT('Ctrl Pts',(46.3726843294707,-16.9165638200946,62.7271778751116));
#3370=CARTESIAN_POINT('Ctrl Pts',(47.0720972607971,-19.8731787510337,63.1181350383136));
#3371=CARTESIAN_POINT('Ctrl Pts',(49.0836136263508,-22.1501399297692,63.5090922015157));
#3372=CARTESIAN_POINT('Ctrl Pts',(51.9314069064712,-23.2088295594817,63.9000493647177));
#3373=CARTESIAN_POINT('Ctrl Pts',(54.9418283114199,-22.7988133854305,64.2910065279198));
#3374=CARTESIAN_POINT('Ctrl Pts',(57.4027591806895,-21.0170812071728,64.6819636911218));
#3375=CARTESIAN_POINT('Ctrl Pts',(58.7320634746702,-18.2851038294562,65.0729208543239));
#3376=CARTESIAN_POINT('Ctrl Pts',(58.6152927272196,-15.2491336565274,65.4638780175259));
#3377=CARTESIAN_POINT('Ctrl Pts',(57.080069193516,-12.6273329394813,65.854835180728));
#3378=CARTESIAN_POINT('Ctrl Pts',(54.4895517737208,-11.039891666206,66.24579234393));
#3379=CARTESIAN_POINT('Ctrl Pts',(51.4565303556175,-10.8623209035087,66.636749507132));
#3380=CARTESIAN_POINT('Ctrl Pts',(48.6984696589939,-12.1366252202991,67.0277066703341));
#3381=CARTESIAN_POINT('Ctrl Pts',(46.8677921271795,-14.5613664587978,67.4186638335361));
#3382=CARTESIAN_POINT('Ctrl Pts',(46.3975466451333,-17.5629692778492,67.8096209967382));
#3383=CARTESIAN_POINT('Ctrl Pts',(47.3989703241477,-20.431401064721,68.2005781599402));
#3384=CARTESIAN_POINT('Ctrl Pts',(49.6351752376468,-22.4881309646939,68.5915353231423));
#3385=CARTESIAN_POINT('Ctrl Pts',(52.5771845274374,-23.2466371494448,68.9824924863443));
#3386=CARTESIAN_POINT('Ctrl Pts',(55.529062504339,-22.5274940937726,69.3734496495464));
#3387=CARTESIAN_POINT('Ctrl Pts',(57.7925390093781,-20.5008159421237,69.7644068127484));
#3388=CARTESIAN_POINT('Ctrl Pts',(58.8321860911263,-17.6460157002987,70.1553639759505));
#3389=CARTESIAN_POINT('Ctrl Pts',(58.4020739661194,-14.6383997751071,70.5463211391525));
#3390=CARTESIAN_POINT('Ctrl Pts',(56.6039462958005,-12.189422944957,70.9372783023545));
#3391=CARTESIAN_POINT('Ctrl Pts',(53.8631519513258,-10.8783940324256,71.3282354655566));
#3392=CARTESIAN_POINT('Ctrl Pts',(50.8280296619087,-11.0154373062825,71.7191926287586));
#3393=CARTESIAN_POINT('Ctrl Pts',(48.2165396770217,-12.5681374761835,72.1101497919607));
#3394=CARTESIAN_POINT('Ctrl Pts',(46.6464360547185,-15.1691962162198,72.5011069551627));
#3395=CARTESIAN_POINT('Ctrl Pts',(46.4891218839111,-18.2033415583671,72.8920641183648));
#3396=CARTESIAN_POINT('Ctrl Pts',(47.7818243197045,-20.9528181004838,73.2830212815669));
#3397=CARTESIAN_POINT('Ctrl Pts',(50.2187210719051,-22.7672877187656,73.6739784447688));
#3398=CARTESIAN_POINT('Ctrl Pts',(53.2234261185118,-23.2174195646428,74.0649356079709));
#3399=CARTESIAN_POINT('Ctrl Pts',(56.085013860659,-22.196986288013,74.4558927711729));
#3400=CARTESIAN_POINT('Ctrl Pts',(58.1268398486099,-19.9468301996286,74.846849934375));
#3401=CARTESIAN_POINT('Ctrl Pts',(58.6189035487885,-17.9825825214271,75.1074880431764));
#3402=CARTESIAN_POINT('Ctrl Pts',(58.6189035487885,-17.,75.237807097577));
#3403=CARTESIAN_POINT('Ctrl Pts',(58.6189035487885,-17.,50.2378070975771));
#3404=CARTESIAN_POINT('Ctrl Pts',(58.6189035487885,-17.0075706036887,50.2948881046132));
#3405=CARTESIAN_POINT('Ctrl Pts',(58.613828368086,-17.0151298524557,50.3518834975562));
#3406=CARTESIAN_POINT('Ctrl Pts',(58.591050565214,-17.0319486181224,50.4786940031426));
#3407=CARTESIAN_POINT('Ctrl Pts',(58.5705467068289,-17.0410922984269,50.5476357284341));
#3408=CARTESIAN_POINT('Ctrl Pts',(58.5425991292395,-17.0498583740029,50.6137303811466));
#3409=CARTESIAN_POINT('Ctrl Pts',(58.4930513356688,-17.0653996029939,50.7309084871288));
#3410=CARTESIAN_POINT('Ctrl Pts',(58.4208808497062,-17.0795128662973,50.8373199854651));
#3411=CARTESIAN_POINT('Ctrl Pts',(58.238833135979,-17.1034494723391,51.0177977431282));
#3412=CARTESIAN_POINT('Ctrl Pts',(58.1304335946722,-17.1130008760904,51.0898136307712));
#3413=CARTESIAN_POINT('Ctrl Pts',(57.8907803690335,-17.1262287645946,51.1895495604053));
#3414=CARTESIAN_POINT('Ctrl Pts',(57.7615831682544,-17.129718953074,51.2158649615548));
#3415=CARTESIAN_POINT('Ctrl Pts',(57.4993934087917,-17.1300465850083,51.2183352481413));
#3416=CARTESIAN_POINT('Ctrl Pts',(57.368745871217,-17.1268329794921,51.1941052333931));
#3417=CARTESIAN_POINT('Ctrl Pts',(57.1245157234726,-17.1140335739622,51.0975999892737));
#3418=CARTESIAN_POINT('Ctrl Pts',(57.0130468177773,-17.1045699914424,51.0262462581385));
#3419=CARTESIAN_POINT('Ctrl Pts',(56.8256541159993,-17.0806911803295,50.8462042639738));
#3420=CARTESIAN_POINT('Ctrl Pts',(56.7510105620165,-17.0665594245304,50.7396533355259));
#3421=CARTESIAN_POINT('Ctrl Pts',(56.6487475381862,-17.0355622762965,50.5059403439088));
#3422=CARTESIAN_POINT('Ctrl Pts',(56.6213788689869,-17.0190611114582,50.3815244925668));
#3423=CARTESIAN_POINT('Ctrl Pts',(56.6189569176101,-17.0015451233,50.2494570532432));
#3424=CARTESIAN_POINT('Ctrl Pts',(56.6189035487885,-17.0007723877109,50.2436307637169));
#3425=CARTESIAN_POINT('Ctrl Pts',(56.6189035487885,-17.,50.2378070975769));
#3426=CARTESIAN_POINT('',(58.6189035487885,-17.,75.237807097577));
#3427=CARTESIAN_POINT('Ctrl Pts',(58.6188665834176,-17.0000025997527,50.237807097577));
#3428=CARTESIAN_POINT('Ctrl Pts',(58.6184633923052,-16.0708764078228,50.3610400036674));
#3429=CARTESIAN_POINT('Ctrl Pts',(58.1676815470056,-14.1595852266855,50.6145919641585));
#3430=CARTESIAN_POINT('Ctrl Pts',(56.2225937043736,-11.897451182557,50.9984629790502));
#3431=CARTESIAN_POINT('Ctrl Pts',(53.3892837467024,-10.8009462068176,51.3894201422522));
#3432=CARTESIAN_POINT('Ctrl Pts',(50.3736273245558,-11.1706588511001,51.7803773054543));
#3433=CARTESIAN_POINT('Ctrl Pts',(47.8891338131767,-12.9193891815025,52.1713344686563));
#3434=CARTESIAN_POINT('Ctrl Pts',(46.523451423545,-15.6333553665913,52.5622916318584));
#3435=CARTESIAN_POINT('Ctrl Pts',(46.599664491672,-18.6706201350726,52.9532487950604));
#3436=CARTESIAN_POINT('Ctrl Pts',(48.0997310899548,-21.3126898076219,53.3442059582625));
#3437=CARTESIAN_POINT('Ctrl Pts',(50.66881515933,-22.9345914086011,53.7351631214646));
#3438=CARTESIAN_POINT('Ctrl Pts',(53.6991939529023,-23.1526568531196,54.1261202846665));
#3439=CARTESIAN_POINT('Ctrl Pts',(56.47402923455,-21.9153050002011,54.5170774478686));
#3440=CARTESIAN_POINT('Ctrl Pts',(58.3369298825998,-19.5152317078047,54.9080346110706));
#3441=CARTESIAN_POINT('Ctrl Pts',(58.8472248890723,-16.5201776181574,55.2989917742727));
#3442=CARTESIAN_POINT('Ctrl Pts',(57.8842032458303,-13.6386259892673,55.6899489374747));
#3443=CARTESIAN_POINT('Ctrl Pts',(55.6756688973336,-11.5522113011612,56.0809061006768));
#3444=CARTESIAN_POINT('Ctrl Pts',(52.7440531658162,-10.7544773055472,56.4718632638789));
#3445=CARTESIAN_POINT('Ctrl Pts',(49.7828331520566,-11.4341289248563,56.8628204270809));
#3446=CARTESIAN_POINT('Ctrl Pts',(47.4924888644779,-13.430393772254,57.253777590283));
#3447=CARTESIAN_POINT('Ctrl Pts',(46.4148038926073,-16.271053097522,57.644734753485));
#3448=CARTESIAN_POINT('Ctrl Pts',(46.8047058599946,-19.2841456537754,58.035691916687));
#3449=CARTESIAN_POINT('Ctrl Pts',(48.5699630065106,-21.7569209176924,58.4266490798891));
#3450=CARTESIAN_POINT('Ctrl Pts',(51.293001714916,-23.1044410439156,58.8176062430911));
#3451=CARTESIAN_POINT('Ctrl Pts',(54.3296840336396,-23.0079485903805,59.2085634062931));
#3452=CARTESIAN_POINT('Ctrl Pts',(56.9616792526266,-21.4902689583137,59.5995205694953));
#3453=CARTESIAN_POINT('Ctrl Pts',(58.5663858627843,-18.9104110177176,59.9904777326972));
#3454=CARTESIAN_POINT('Ctrl Pts',(58.7642086619611,-15.8786431442651,60.3814348958993));
#3455=CARTESIAN_POINT('Ctrl Pts',(57.5083524385236,-13.112133530256,60.7723920591013));
#3456=CARTESIAN_POINT('Ctrl Pts',(55.095891432692,-11.2653032203185,61.1633492223034));
#3457=CARTESIAN_POINT('Ctrl Pts',(52.0974960818944,-10.77502205744,61.5543063855054));
#3458=CARTESIAN_POINT('Ctrl Pts',(49.2224402696388,-11.7572666169945,61.9452635487075));
#3459=CARTESIAN_POINT('Ctrl Pts',(47.1508217691292,-13.9796858138845,62.3362207119095));
#3460=CARTESIAN_POINT('Ctrl Pts',(46.3726843294707,-16.9165638200946,62.7271778751116));
#3461=CARTESIAN_POINT('Ctrl Pts',(47.0720972607971,-19.8731787510337,63.1181350383136));
#3462=CARTESIAN_POINT('Ctrl Pts',(49.0836136263508,-22.1501399297692,63.5090922015157));
#3463=CARTESIAN_POINT('Ctrl Pts',(51.9314069064712,-23.2088295594817,63.9000493647177));
#3464=CARTESIAN_POINT('Ctrl Pts',(54.9418283114199,-22.7988133854305,64.2910065279198));
#3465=CARTESIAN_POINT('Ctrl Pts',(57.4027591806895,-21.0170812071728,64.6819636911218));
#3466=CARTESIAN_POINT('Ctrl Pts',(58.7320634746702,-18.2851038294562,65.0729208543239));
#3467=CARTESIAN_POINT('Ctrl Pts',(58.6152927272196,-15.2491336565274,65.4638780175259));
#3468=CARTESIAN_POINT('Ctrl Pts',(57.080069193516,-12.6273329394813,65.854835180728));
#3469=CARTESIAN_POINT('Ctrl Pts',(54.4895517737208,-11.039891666206,66.24579234393));
#3470=CARTESIAN_POINT('Ctrl Pts',(51.4565303556175,-10.8623209035087,66.636749507132));
#3471=CARTESIAN_POINT('Ctrl Pts',(48.6984696589939,-12.1366252202991,67.0277066703341));
#3472=CARTESIAN_POINT('Ctrl Pts',(46.8677921271795,-14.5613664587978,67.4186638335361));
#3473=CARTESIAN_POINT('Ctrl Pts',(46.3975466451333,-17.5629692778492,67.8096209967382));
#3474=CARTESIAN_POINT('Ctrl Pts',(47.3989703241477,-20.431401064721,68.2005781599402));
#3475=CARTESIAN_POINT('Ctrl Pts',(49.6351752376468,-22.4881309646939,68.5915353231423));
#3476=CARTESIAN_POINT('Ctrl Pts',(52.5771845274374,-23.2466371494448,68.9824924863443));
#3477=CARTESIAN_POINT('Ctrl Pts',(55.529062504339,-22.5274940937726,69.3734496495464));
#3478=CARTESIAN_POINT('Ctrl Pts',(57.7925390093781,-20.5008159421237,69.7644068127484));
#3479=CARTESIAN_POINT('Ctrl Pts',(58.8321860911263,-17.6460157002987,70.1553639759505));
#3480=CARTESIAN_POINT('Ctrl Pts',(58.4020739661194,-14.6383997751071,70.5463211391525));
#3481=CARTESIAN_POINT('Ctrl Pts',(56.6039462958005,-12.189422944957,70.9372783023545));
#3482=CARTESIAN_POINT('Ctrl Pts',(53.8631519513258,-10.8783940324256,71.3282354655566));
#3483=CARTESIAN_POINT('Ctrl Pts',(50.8280296619087,-11.0154373062825,71.7191926287586));
#3484=CARTESIAN_POINT('Ctrl Pts',(48.2165396770217,-12.5681374761835,72.1101497919607));
#3485=CARTESIAN_POINT('Ctrl Pts',(46.6464360547185,-15.1691962162198,72.5011069551627));
#3486=CARTESIAN_POINT('Ctrl Pts',(46.4891218839111,-18.2033415583671,72.8920641183648));
#3487=CARTESIAN_POINT('Ctrl Pts',(47.7818243197045,-20.9528181004838,73.2830212815669));
#3488=CARTESIAN_POINT('Ctrl Pts',(50.2187210719051,-22.7672877187656,73.6739784447688));
#3489=CARTESIAN_POINT('Ctrl Pts',(53.2234261185118,-23.2174195646428,74.0649356079709));
#3490=CARTESIAN_POINT('Ctrl Pts',(56.085013860659,-22.196986288013,74.4558927711729));
#3491=CARTESIAN_POINT('Ctrl Pts',(58.1268398486099,-19.9468301996286,74.846849934375));
#3492=CARTESIAN_POINT('Ctrl Pts',(58.6189035487885,-17.9825825214271,75.1074880431764));
#3493=CARTESIAN_POINT('Ctrl Pts',(58.6189035487885,-17.,75.237807097577));
#3494=CARTESIAN_POINT('',(56.6189035487885,-17.,75.2378070975771));
#3495=CARTESIAN_POINT('Ctrl Pts',(58.6189035487885,-17.,75.237807097577));
#3496=CARTESIAN_POINT('Ctrl Pts',(58.6189035487885,-17.008960117349,75.3053647907907));
#3497=CARTESIAN_POINT('Ctrl Pts',(58.6117944887821,-17.0178948508948,75.3727310946367));
#3498=CARTESIAN_POINT('Ctrl Pts',(58.5835895459723,-17.0354327396429,75.5049636605181));
#3499=CARTESIAN_POINT('Ctrl Pts',(58.5625652615718,-17.0439860715606,75.5694542638574));
#3500=CARTESIAN_POINT('Ctrl Pts',(58.4828049675281,-17.0676897484131,75.7481757768082));
#3501=CARTESIAN_POINT('Ctrl Pts',(58.4079637983781,-17.0816898329777,75.8537339275911));
#3502=CARTESIAN_POINT('Ctrl Pts',(58.2206375760899,-17.1052702229138,76.0315258790922));
#3503=CARTESIAN_POINT('Ctrl Pts',(58.1096236898478,-17.1145665084967,76.1016182210869));
#3504=CARTESIAN_POINT('Ctrl Pts',(57.8656078740837,-17.1271089995502,76.1961863756905));
#3505=CARTESIAN_POINT('Ctrl Pts',(57.7347565193837,-17.1301779251459,76.2193255295076));
#3506=CARTESIAN_POINT('Ctrl Pts',(57.4713951509218,-17.1295550490469,76.2146291543638));
#3507=CARTESIAN_POINT('Ctrl Pts',(57.3412656322973,-17.1258605590003,76.1867733556523));
#3508=CARTESIAN_POINT('Ctrl Pts',(57.1006247689232,-17.1122064533128,76.0838238241662));
#3509=CARTESIAN_POINT('Ctrl Pts',(56.9919980123763,-17.1024344565023,76.0101447038231));
#3510=CARTESIAN_POINT('Ctrl Pts',(56.8111979530795,-17.0781956792231,75.8273886287054));
#3511=CARTESIAN_POINT('Ctrl Pts',(56.7400261926721,-17.064034548912,75.7206162211305));
#3512=CARTESIAN_POINT('Ctrl Pts',(56.6436413373651,-17.0330811637281,75.4872331951366));
#3513=CARTESIAN_POINT('Ctrl Pts',(56.6189035487885,-17.0166298921152,75.3631935301346));
#3514=CARTESIAN_POINT('Ctrl Pts',(56.6189035487885,-17.,75.2378070975771));
#3515=CARTESIAN_POINT('',(56.7160709287438,-17.0505280490765,74.7973480456327));
#3516=CARTESIAN_POINT('Ctrl Pts',(56.619807216532,-17.,75.2373164241775));
#3517=CARTESIAN_POINT('Ctrl Pts',(56.6197919231519,-17.0008600414084,75.22926047205));
#3518=CARTESIAN_POINT('Ctrl Pts',(56.6198658096928,-17.0017200514272,75.2212050523955));
#3519=CARTESIAN_POINT('Ctrl Pts',(56.6200289121166,-17.0025803567058,75.2131518394368));
#3520=CARTESIAN_POINT('Ctrl Pts',(56.6209590323085,-17.0074863985172,75.1672269794184));
#3521=CARTESIAN_POINT('Ctrl Pts',(56.6247833784199,-17.0123852229216,75.1215182732402));
#3522=CARTESIAN_POINT('Ctrl Pts',(56.6314848898377,-17.0173394870174,75.0763314642167));
#3523=CARTESIAN_POINT('Ctrl Pts',(56.6380508197605,-17.0221935190177,75.0320588512208));
#3524=CARTESIAN_POINT('Ctrl Pts',(56.6473788385076,-17.027100631373,74.9882860750618));
#3525=CARTESIAN_POINT('Ctrl Pts',(56.659501419885,-17.0321210350159,74.9453059975962));
#3526=CARTESIAN_POINT('Ctrl Pts',(56.6674796286738,-17.0354251026249,74.9170196103077));
#3527=CARTESIAN_POINT('Ctrl Pts',(56.6766692322283,-17.0387782700352,74.8890767068547));
#3528=CARTESIAN_POINT('Ctrl Pts',(56.6870908888333,-17.0421984494337,74.8615656693999));
#3529=CARTESIAN_POINT('Ctrl Pts',(56.6954202403711,-17.0449319761283,74.8395778884914));
#3530=CARTESIAN_POINT('Ctrl Pts',(56.7045106227115,-17.0477003616562,74.8179350323125));
#3531=CARTESIAN_POINT('Ctrl Pts',(56.7143627134912,-17.0505136943971,74.7966769441347));
#3532=CARTESIAN_POINT('',(57.0485964548729,-16.9999999999999,74.4163755309633));
#3533=CARTESIAN_POINT('Ctrl Pts',(56.7160709287427,-17.0505280490768,74.7973480456349));
#3534=CARTESIAN_POINT('Ctrl Pts',(56.734112437174,-17.0456614403176,74.7606546800529));
#3535=CARTESIAN_POINT('Ctrl Pts',(56.7545070450986,-17.0409383108094,74.7250431225245));
#3536=CARTESIAN_POINT('Ctrl Pts',(56.8485610192468,-17.0220366934414,74.5825282850899));
#3537=CARTESIAN_POINT('Ctrl Pts',(56.9409174602205,-17.0096845848757,74.4893955806398));
#3538=CARTESIAN_POINT('Ctrl Pts',(57.048596454873,-17.,74.4163755309633));
#3539=CARTESIAN_POINT('',(58.1892106427041,-17.,74.4163755309633));
#3540=CARTESIAN_POINT('Origin',(57.6189035487885,-17.,75.237807097577));
#3541=CARTESIAN_POINT('Origin',(57.6189035487885,-17.,75.237807097577));
#3542=CARTESIAN_POINT('Ctrl Pts',(58.6189035487885,-17.,50.237807097577));
#3543=CARTESIAN_POINT('Ctrl Pts',(58.6189035487885,-16.991039882651,50.1702494043634));
#3544=CARTESIAN_POINT('Ctrl Pts',(58.6117944887821,-16.9821051491052,50.1028831005174));
#3545=CARTESIAN_POINT('Ctrl Pts',(58.5835895459723,-16.9645672603571,49.9706505346359));
#3546=CARTESIAN_POINT('Ctrl Pts',(58.5625652615718,-16.9560139284394,49.9061599312966));
#3547=CARTESIAN_POINT('Ctrl Pts',(58.4828049675281,-16.9323102515869,49.7274384183459));
#3548=CARTESIAN_POINT('Ctrl Pts',(58.4079637983781,-16.9183101670223,49.6218802675629));
#3549=CARTESIAN_POINT('Ctrl Pts',(58.2206375760899,-16.8947297770862,49.4440883160619));
#3550=CARTESIAN_POINT('Ctrl Pts',(58.1096236898478,-16.8854334915033,49.3739959740672));
#3551=CARTESIAN_POINT('Ctrl Pts',(57.8656078740836,-16.8728910004498,49.2794278194636));
#3552=CARTESIAN_POINT('Ctrl Pts',(57.7347565193837,-16.8698220748541,49.2562886656465));
#3553=CARTESIAN_POINT('Ctrl Pts',(57.4713951509218,-16.8704449509531,49.2609850407903));
#3554=CARTESIAN_POINT('Ctrl Pts',(57.3412656322973,-16.8741394409997,49.2888408395018));
#3555=CARTESIAN_POINT('Ctrl Pts',(57.1006247689232,-16.8877935466872,49.3917903709879));
#3556=CARTESIAN_POINT('Ctrl Pts',(56.9919980123763,-16.8975655434977,49.465469491331));
#3557=CARTESIAN_POINT('Ctrl Pts',(56.8111979530794,-16.9218043207769,49.6482255664488));
#3558=CARTESIAN_POINT('Ctrl Pts',(56.740026192672,-16.935965451088,49.7549979740236));
#3559=CARTESIAN_POINT('Ctrl Pts',(56.6436413373651,-16.9669188362719,49.9883810000176));
#3560=CARTESIAN_POINT('Ctrl Pts',(56.6189035487885,-16.9833701078848,50.1124206650196));
#3561=CARTESIAN_POINT('Ctrl Pts',(56.6189035487885,-17.,50.237807097577));
#3562=CARTESIAN_POINT('Origin',(57.6189035487885,-17.15,50.237807097577));
#3563=CARTESIAN_POINT('Ctrl Pts',(57.0353881436569,-17.1499999999404,49.3968642735725));
#3564=CARTESIAN_POINT('Ctrl Pts',(56.9995277725034,-17.1500003183691,49.4222269403983));
#3565=CARTESIAN_POINT('Ctrl Pts',(56.9653733978866,-17.1500025402159,49.4500582165395));
#3566=CARTESIAN_POINT('Ctrl Pts',(56.9331114218803,-17.1500046663948,49.4801422563167));
#3567=CARTESIAN_POINT('Ctrl Pts',(56.9007444405485,-17.1500067994939,49.5103242127372));
#3568=CARTESIAN_POINT('Ctrl Pts',(56.8704989342592,-17.1500088846928,49.5425711070994));
#3569=CARTESIAN_POINT('Ctrl Pts',(56.842517628275,-17.1500096437477,49.576616148902));
#3570=CARTESIAN_POINT('Ctrl Pts',(56.8144621758977,-17.1500104048139,49.6107514051163));
#3571=CARTESIAN_POINT('Ctrl Pts',(56.7886822426408,-17.1500098407062,49.646695273018));
#3572=CARTESIAN_POINT('Ctrl Pts',(56.7653583390214,-17.1500083475778,49.6842152192191));
#3573=CARTESIAN_POINT('Ctrl Pts',(56.7440381590042,-17.1500069827219,49.7185118798595));
#3574=CARTESIAN_POINT('Ctrl Pts',(56.7247701610183,-17.1500048688239,49.7541263894184));
#3575=CARTESIAN_POINT('Ctrl Pts',(56.7077264766587,-17.1500034254948,49.7908978528519));
#3576=CARTESIAN_POINT('Ctrl Pts',(56.6967102134416,-17.1500024925924,49.8146652561618));
#3577=CARTESIAN_POINT('Ctrl Pts',(56.6866679969386,-17.1500013277767,49.8388214631241));
#3578=CARTESIAN_POINT('Ctrl Pts',(56.6776310476167,-17.1500011365132,49.863315773977));
#3579=CARTESIAN_POINT('Ctrl Pts',(56.6624572664577,-17.150000815366,49.9044437364435));
#3580=CARTESIAN_POINT('Ctrl Pts',(56.650114799487,-17.1500032648176,49.9465239883955));
#3581=CARTESIAN_POINT('Ctrl Pts',(56.640580505364,-17.1500062417895,49.9892605406622));
#3582=CARTESIAN_POINT('Ctrl Pts',(56.6309401368815,-17.150009251882,50.0324725609973));
#3583=CARTESIAN_POINT('Ctrl Pts',(56.624170610253,-17.1500128171849,50.0763567021812));
#3584=CARTESIAN_POINT('Ctrl Pts',(56.6202990237812,-17.1500140834455,50.1206190671135));
#3585=CARTESIAN_POINT('Ctrl Pts',(56.6190338326219,-17.1500144972454,50.1350835129449));
#3586=CARTESIAN_POINT('Ctrl Pts',(56.6180785278747,-17.1500146602173,50.1495883714516));
#3587=CARTESIAN_POINT('Ctrl Pts',(56.6174352663666,-17.1500144553777,50.1641233425841));
#3588=CARTESIAN_POINT('Ctrl Pts',(56.6154669730407,-17.150013828596,50.2085983909243));
#3589=CARTESIAN_POINT('Ctrl Pts',(56.6164293147499,-17.1500098830758,50.2530643615513));
#3590=CARTESIAN_POINT('Ctrl Pts',(56.6203035167127,-17.1500063372223,50.2972233337701));
#3591=CARTESIAN_POINT('Ctrl Pts',(56.6241712235008,-17.1500027973134,50.3413082726175));
#3592=CARTESIAN_POINT('Ctrl Pts',(56.6309410033718,-17.1499996436082,50.3850883978143));
#3593=CARTESIAN_POINT('Ctrl Pts',(56.6406452513128,-17.1499996640019,50.4282695972847));
#3594=CARTESIAN_POINT('Ctrl Pts',(56.6424167756711,-17.1499996677248,50.4361523870845));
#3595=CARTESIAN_POINT('Ctrl Pts',(56.6442862295108,-17.1499997750282,50.4440151968179));
#3596=CARTESIAN_POINT('Ctrl Pts',(56.6462539958365,-17.1499999999996,50.4518561987028));
#3597=CARTESIAN_POINT('Origin',(57.6189035487885,-17.,75.237807097577));
#3598=CARTESIAN_POINT('',(58.1993466393407,-17.,74.4163755309629));
#3599=CARTESIAN_POINT('',(57.6189035487885,-17.,74.4163755309633));
#3600=CARTESIAN_POINT('Ctrl Pts',(58.1997282611953,-16.9998571535648,74.4152984942148));
#3601=CARTESIAN_POINT('Ctrl Pts',(58.2143357917363,-16.9998440707738,74.4257197573308));
#3602=CARTESIAN_POINT('Ctrl Pts',(58.2286519425552,-16.9998332935578,74.4365601307609));
#3603=CARTESIAN_POINT('Ctrl Pts',(58.2426546458167,-16.9998261318276,74.4478189175199));
#3604=CARTESIAN_POINT('Ctrl Pts',(58.2570875587164,-16.9998187500652,74.4594236116718));
#3605=CARTESIAN_POINT('Ctrl Pts',(58.271187472638,-16.9998152116138,74.4714728412125));
#3606=CARTESIAN_POINT('Ctrl Pts',(58.2849450357921,-16.9998144462796,74.4839469418765));
#3607=CARTESIAN_POINT('Ctrl Pts',(58.3171667594867,-16.999812653783,74.5131626554759));
#3608=CARTESIAN_POINT('Ctrl Pts',(58.3473079189655,-16.9998260898473,74.544520126789));
#3609=CARTESIAN_POINT('Ctrl Pts',(58.3753004444692,-16.9998438498395,74.5777107138075));
#3610=CARTESIAN_POINT('Ctrl Pts',(58.4041614873196,-16.9998621608667,74.6119310971753));
#3611=CARTESIAN_POINT('Ctrl Pts',(58.4307391732154,-16.9998851867719,74.6481009779077));
#3612=CARTESIAN_POINT('Ctrl Pts',(58.4549224048529,-16.9999065586214,74.685924045946));
#3613=CARTESIAN_POINT('Ctrl Pts',(58.4775163765478,-16.9999265259678,74.7212614789856));
#3614=CARTESIAN_POINT('Ctrl Pts',(58.4980202826146,-16.9999452002503,74.7580430626991));
#3615=CARTESIAN_POINT('Ctrl Pts',(58.5163082288499,-16.9999601156304,74.7960480062526));
#3616=CARTESIAN_POINT('Ctrl Pts',(58.5359309705969,-16.9999761196501,74.8368268440109));
#3617=CARTESIAN_POINT('Ctrl Pts',(58.5528792611933,-16.9999879520546,74.8787568015286));
#3618=CARTESIAN_POINT('Ctrl Pts',(58.5670508442818,-16.9999950681616,74.9215394899968));
#3619=CARTESIAN_POINT('Ctrl Pts',(58.5810408703955,-17.0000020931016,74.9637740748802));
#3620=CARTESIAN_POINT('Ctrl Pts',(58.5923252734734,-17.000004670778,75.0068407878673));
#3621=CARTESIAN_POINT('Ctrl Pts',(58.600760876798,-17.0000048908046,75.0504735477835));
#3622=CARTESIAN_POINT('Ctrl Pts',(58.6087537841981,-17.0000050992843,75.0918164839313));
#3623=CARTESIAN_POINT('Ctrl Pts',(58.6141890828729,-17.0000033086596,75.1336685099678));
#3624=CARTESIAN_POINT('Ctrl Pts',(58.6169020048606,-17.0000017472687,75.175807863164));
#3625=CARTESIAN_POINT('Ctrl Pts',(58.6182322861701,-17.0000009816407,75.1964708952038));
#3626=CARTESIAN_POINT('Ctrl Pts',(58.6189035487885,-16.999997221476,75.2171455663987));
#3627=CARTESIAN_POINT('Ctrl Pts',(58.6189035487885,-17.0000000161406,75.2378038846518));
#3628=CARTESIAN_POINT('Ctrl Pts',(58.6189035487885,-17.1070624647046,75.2236074971792));
#3629=CARTESIAN_POINT('Ctrl Pts',(58.6189035487885,-17.0713749764698,75.2283406973118));
#3630=CARTESIAN_POINT('Ctrl Pts',(58.6189035487885,-17.0356873793413,75.2330738853036));
#3631=CARTESIAN_POINT('Ctrl Pts',(58.6189035487885,-16.868940610655,75.2551744844083));
#3632=CARTESIAN_POINT('Ctrl Pts',(58.6189035487886,-16.6072943602623,75.2878910531892));
#3633=CARTESIAN_POINT('Ctrl Pts',(58.6189035487885,-16.0863108570333,75.3474872987329));
#3634=CARTESIAN_POINT('Ctrl Pts',(58.6189035487885,-15.4407089605501,75.4198407374667));
#3635=CARTESIAN_POINT('Ctrl Pts',(58.6189035487886,-14.810515552782,75.530562741844));
#3636=CARTESIAN_POINT('Ctrl Pts',(58.6189035487885,-14.3226785985763,75.6740330751718));
#3637=CARTESIAN_POINT('Ctrl Pts',(58.6189035487886,-13.6119901077366,75.9531021796814));
#3638=CARTESIAN_POINT('Ctrl Pts',(58.6189035487885,-12.6391386971879,76.6898853504872));
#3639=CARTESIAN_POINT('Ctrl Pts',(58.6189035487886,-11.9421053181931,77.9551448661809));
#3640=CARTESIAN_POINT('Ctrl Pts',(58.6189035487886,-11.620123611833,78.904610366011));
#3641=CARTESIAN_POINT('Ctrl Pts',(58.6189035487886,-11.4414090651326,79.5566822517067));
#3642=CARTESIAN_POINT('Ctrl Pts',(58.6189035487886,-11.283611680672,80.3904836204666));
#3643=CARTESIAN_POINT('Ctrl Pts',(58.6189035487885,-11.191771906312,81.2094324300899));
#3644=CARTESIAN_POINT('Ctrl Pts',(58.6189035487885,-11.1351578812696,81.8374901150816));
#3645=CARTESIAN_POINT('Ctrl Pts',(58.6189035487885,-11.053369822089,82.7460850644104));
#3646=CARTESIAN_POINT('Ctrl Pts',(58.6189035487885,-10.9236831233095,83.6860531538696));
#3647=CARTESIAN_POINT('Ctrl Pts',(58.6189035487885,-10.4992473440377,84.5353425071605));
#3648=CARTESIAN_POINT('Ctrl Pts',(58.6189035487886,-10.0852341421502,84.9682405076987));
#3649=CARTESIAN_POINT('Ctrl Pts',(58.6189035487886,-9.65205447547462,85.2538515396933));
#3650=CARTESIAN_POINT('Ctrl Pts',(58.6189035487886,-9.1488264052405,85.4990822689984));
#3651=CARTESIAN_POINT('Ctrl Pts',(58.6189035487885,-8.07907491053992,85.8217946659718));
#3652=CARTESIAN_POINT('Ctrl Pts',(58.6189035487885,-6.83128625461351,85.9175112317093));
#3653=CARTESIAN_POINT('Ctrl Pts',(58.6189035487885,-5.85324890998301,85.9023446784181));
#3654=CARTESIAN_POINT('Ctrl Pts',(58.6189035487885,-17.0677244044812,74.9270055107683));
#3655=CARTESIAN_POINT('Ctrl Pts',(58.6189035487885,-17.0320369162463,74.9317387109009));
#3656=CARTESIAN_POINT('Ctrl Pts',(58.6189035487885,-16.9963437059072,74.9364726710977));
#3657=CARTESIAN_POINT('Ctrl Pts',(58.6189035487885,-16.8296431542228,74.9585653195626));
#3658=CARTESIAN_POINT('Ctrl Pts',(58.6189035487886,-16.5713180684596,74.990859086523));
#3659=CARTESIAN_POINT('Ctrl Pts',(58.6189035487885,-16.0526651090702,75.050198376707));
#3660=CARTESIAN_POINT('Ctrl Pts',(58.6189035487885,-15.40137640994,75.1231150129893));
#3661=CARTESIAN_POINT('Ctrl Pts',(58.6189035487886,-14.7450284330187,75.2377433098845));
#3662=CARTESIAN_POINT('Ctrl Pts',(58.6189035487885,-14.2255085991446,75.3905130433138));
#3663=CARTESIAN_POINT('Ctrl Pts',(58.6189035487886,-13.4573378756898,75.691187535415));
#3664=CARTESIAN_POINT('Ctrl Pts',(58.6189035487885,-12.3965385704437,76.4991688124884));
#3665=CARTESIAN_POINT('Ctrl Pts',(58.6189035487886,-11.6684548706516,77.8319408520014));
#3666=CARTESIAN_POINT('Ctrl Pts',(58.6189035487886,-11.3339319292239,78.8171580204204));
#3667=CARTESIAN_POINT('Ctrl Pts',(58.6189035487886,-11.1493868708181,79.4910278264843));
#3668=CARTESIAN_POINT('Ctrl Pts',(58.6189035487886,-10.9873493355326,80.347370825992));
#3669=CARTESIAN_POINT('Ctrl Pts',(58.6189035487885,-10.8941820327677,81.1800702256411));
#3670=CARTESIAN_POINT('Ctrl Pts',(58.6189035487885,-10.8371602227307,81.8111085619185));
#3671=CARTESIAN_POINT('Ctrl Pts',(58.6189035487885,-10.7562651177072,82.7152910391538));
#3672=CARTESIAN_POINT('Ctrl Pts',(58.6189035487885,-10.62680068035,83.6154368879388));
#3673=CARTESIAN_POINT('Ctrl Pts',(58.6189035487885,-10.2493987285943,84.3618958202144));
#3674=CARTESIAN_POINT('Ctrl Pts',(58.6189035487886,-9.8919152225634,84.7369092153924));
#3675=CARTESIAN_POINT('Ctrl Pts',(58.6189035487886,-9.50503348466235,84.9925351153733));
#3676=CARTESIAN_POINT('Ctrl Pts',(58.6189035487886,-9.04537663272557,85.2168574142422));
#3677=CARTESIAN_POINT('Ctrl Pts',(58.6189035487885,-8.0378464978853,85.5227638874191));
#3678=CARTESIAN_POINT('Ctrl Pts',(58.6189035487885,-6.82025743271601,85.6181049337487));
#3679=CARTESIAN_POINT('Ctrl Pts',(58.6189035487885,-5.85788807498938,85.603181345984));
#3680=CARTESIAN_POINT('Ctrl Pts',(58.3322714066286,-16.9892828575829,74.3355701808357));
#3681=CARTESIAN_POINT('Ctrl Pts',(58.3322714066286,-16.953595369348,74.3403033809683));
#3682=CARTESIAN_POINT('Ctrl Pts',(58.3322714066287,-16.9178909302647,74.3450389025498));
#3683=CARTESIAN_POINT('Ctrl Pts',(58.3322714066286,-16.7512842541308,74.3671145332137));
#3684=CARTESIAN_POINT('Ctrl Pts',(58.3322714066287,-16.499588634895,74.3985624655087));
#3685=CARTESIAN_POINT('Ctrl Pts',(58.3322714066286,-15.9855939784622,74.4573831305653));
#3686=CARTESIAN_POINT('Ctrl Pts',(58.3322714066287,-15.3229750899196,74.5314130013934));
#3687=CARTESIAN_POINT('Ctrl Pts',(58.3322714066287,-14.6144661000659,74.6538202774898));
#3688=CARTESIAN_POINT('Ctrl Pts',(58.3322714066287,-14.0317403735836,74.8251403710485));
#3689=CARTESIAN_POINT('Ctrl Pts',(58.3322714066287,-13.148909444107,75.1689004861853));
#3690=CARTESIAN_POINT('Ctrl Pts',(58.3322714066286,-11.9126649225552,76.1189177484811));
#3691=CARTESIAN_POINT('Ctrl Pts',(58.3322714066287,-11.1227142479736,77.5862953260158));
#3692=CARTESIAN_POINT('Ctrl Pts',(58.3322714066287,-10.7631722715652,78.642838701811));
#3693=CARTESIAN_POINT('Ctrl Pts',(58.3322714066287,-10.5669977147391,79.3601938732302));
#3694=CARTESIAN_POINT('Ctrl Pts',(58.3322714066287,-10.3965037381347,80.2615040278716));
#3695=CARTESIAN_POINT('Ctrl Pts',(58.3322714066286,-10.3006886617217,81.1216343338287));
#3696=CARTESIAN_POINT('Ctrl Pts',(58.3322714066286,-10.2428505130289,81.7586216789515));
#3697=CARTESIAN_POINT('Ctrl Pts',(58.3322714066286,-10.1637401686721,82.6539973819218));
#3698=CARTESIAN_POINT('Ctrl Pts',(58.3322714066287,-10.0346447578536,83.4747687679503));
#3699=CARTESIAN_POINT('Ctrl Pts',(58.3322714066287,-9.75107986379657,84.0160716707905));
#3700=CARTESIAN_POINT('Ctrl Pts',(58.3322714066287,-9.50634793399624,84.2756235640084));
#3701=CARTESIAN_POINT('Ctrl Pts',(58.3322714066287,-9.2118265761089,84.4714332158408));
#3702=CARTESIAN_POINT('Ctrl Pts',(58.3322714066287,-8.83908636867753,84.6540485794195));
#3703=CARTESIAN_POINT('Ctrl Pts',(58.3322714066287,-7.9556774348701,84.9264368884188));
#3704=CARTESIAN_POINT('Ctrl Pts',(58.3322714066286,-6.79824855322479,85.0210774392432));
#3705=CARTESIAN_POINT('Ctrl Pts',(58.3322714066286,-5.86713874157915,85.0066385973567));
#3706=CARTESIAN_POINT('Ctrl Pts',(57.3646226285175,-16.9604946724078,74.1185123783007));
#3707=CARTESIAN_POINT('Ctrl Pts',(57.3646226285175,-16.9248071841729,74.1232455784333));
#3708=CARTESIAN_POINT('Ctrl Pts',(57.3646226285175,-16.889098333514,74.1279818482412));
#3709=CARTESIAN_POINT('Ctrl Pts',(57.3646226285175,-16.7225400508609,74.1500417837015));
#3710=CARTESIAN_POINT('Ctrl Pts',(57.3646226285175,-16.4733338130514,74.1811569488366));
#3711=CARTESIAN_POINT('Ctrl Pts',(57.3646226285175,-15.9611389801221,74.2397365628143));
#3712=CARTESIAN_POINT('Ctrl Pts',(57.3646226285175,-15.2944390637735,74.3140954113275));
#3713=CARTESIAN_POINT('Ctrl Pts',(57.3646226285175,-14.5667232822858,74.4392738616914));
#3714=CARTESIAN_POINT('Ctrl Pts',(57.3646226285175,-13.9605649616208,74.6174589018033));
#3715=CARTESIAN_POINT('Ctrl Pts',(57.3646226285176,-13.0353408967044,74.9770614024389));
#3716=CARTESIAN_POINT('Ctrl Pts',(57.3646226285175,-11.7341080097852,75.9797283837915));
#3717=CARTESIAN_POINT('Ctrl Pts',(57.3646226285176,-10.9218459124412,77.4963689695129));
#3718=CARTESIAN_POINT('Ctrl Pts',(57.3646226285176,-10.5530297713597,78.5793819337369));
#3719=CARTESIAN_POINT('Ctrl Pts',(57.3646226285175,-10.3525608436317,79.312854674376));
#3720=CARTESIAN_POINT('Ctrl Pts',(57.3646226285176,-10.1789517790958,80.2308165058766));
#3721=CARTESIAN_POINT('Ctrl Pts',(57.3646226285175,-10.0821598266619,81.1011091643012));
#3722=CARTESIAN_POINT('Ctrl Pts',(57.3646226285175,-10.023996097922,81.7403242963189));
#3723=CARTESIAN_POINT('Ctrl Pts',(57.3646226285175,-9.94557467621999,82.6324017972352));
#3724=CARTESIAN_POINT('Ctrl Pts',(57.3646226285175,-9.81601252498804,83.4243069447849));
#3725=CARTESIAN_POINT('Ctrl Pts',(57.3646226285175,-9.56729084574229,83.8894374229533));
#3726=CARTESIAN_POINT('Ctrl Pts',(57.3646226285175,-9.36417659416019,84.1063106299724));
#3727=CARTESIAN_POINT('Ctrl Pts',(57.3646226285175,-9.10388126033771,84.2799663831815));
#3728=CARTESIAN_POINT('Ctrl Pts',(57.3646226285175,-8.76331584417413,84.4471554629121));
#3729=CARTESIAN_POINT('Ctrl Pts',(57.3646226285175,-7.92586155372296,84.7071895267139));
#3730=CARTESIAN_POINT('Ctrl Pts',(57.3646226285175,-6.79003323137325,84.8019651621459));
#3731=CARTESIAN_POINT('Ctrl Pts',(57.3646226285175,-5.87053375242876,84.7877063632102));
#3732=CARTESIAN_POINT('Ctrl Pts',(56.5859422264137,-17.0417044640364,74.7308197817729));
#3733=CARTESIAN_POINT('Ctrl Pts',(56.5859422264137,-17.0060169758015,74.7355529819055));
#3734=CARTESIAN_POINT('Ctrl Pts',(56.5859422264137,-16.9703200156519,74.7402874751691));
#3735=CARTESIAN_POINT('Ctrl Pts',(56.5859422264137,-16.8036518081296,74.7623736621299));
#3736=CARTESIAN_POINT('Ctrl Pts',(56.5859422264137,-16.5475306602109,74.7943849255561));
#3737=CARTESIAN_POINT('Ctrl Pts',(56.5859422264137,-16.0304307075519,74.8535477998962));
#3738=CARTESIAN_POINT('Ctrl Pts',(56.5859422264137,-15.3753903256926,74.926826832225));
#3739=CARTESIAN_POINT('Ctrl Pts',(56.5859422264137,-14.7017344598755,75.0440282693776));
#3740=CARTESIAN_POINT('Ctrl Pts',(56.5859422264137,-14.1612281378247,75.2029562844881));
#3741=CARTESIAN_POINT('Ctrl Pts',(56.5859422264137,-13.3549963246989,75.517925343114));
#3742=CARTESIAN_POINT('Ctrl Pts',(56.5859422264136,-12.2359480597188,76.3730666756037));
#3743=CARTESIAN_POINT('Ctrl Pts',(56.5859422264138,-11.4873764233173,77.7504770035942));
#3744=CARTESIAN_POINT('Ctrl Pts',(56.5859422264137,-11.1445464264738,78.7593791696242));
#3745=CARTESIAN_POINT('Ctrl Pts',(56.5859422264137,-10.9561414584619,79.4476872424981));
#3746=CARTESIAN_POINT('Ctrl Pts',(56.5859422264137,-10.7912978280097,80.3189591959352));
#3747=CARTESIAN_POINT('Ctrl Pts',(56.5859422264137,-10.6972517850491,81.1607659572902));
#3748=CARTESIAN_POINT('Ctrl Pts',(56.5859422264137,-10.6399569412909,81.7937814907276));
#3749=CARTESIAN_POINT('Ctrl Pts',(56.5859422264137,-10.5596567916307,82.6950369507156));
#3750=CARTESIAN_POINT('Ctrl Pts',(56.5859422264137,-10.4302627328852,83.5688762400591));
#3751=CARTESIAN_POINT('Ctrl Pts',(56.5859422264137,-10.0840225667115,84.2472065970568));
#3752=CARTESIAN_POINT('Ctrl Pts',(56.5859422264137,-9.76396055712458,84.5838938404408));
#3753=CARTESIAN_POINT('Ctrl Pts',(56.5859422264137,-9.40774427240785,84.8196606327552));
#3754=CARTESIAN_POINT('Ctrl Pts',(56.5859422264137,-8.97694251385567,85.0301379251509));
#3755=CARTESIAN_POINT('Ctrl Pts',(56.5859422264137,-8.01061950340817,85.3249214662463));
#3756=CARTESIAN_POINT('Ctrl Pts',(56.5859422264137,-6.81294491447546,85.4200640361347));
#3757=CARTESIAN_POINT('Ctrl Pts',(56.5859422264137,-5.86095662479822,85.4053014289528));
#3758=CARTESIAN_POINT('Ctrl Pts',(56.5889518727976,-17.1722671939372,75.7152395731868));
#3759=CARTESIAN_POINT('Ctrl Pts',(56.5889518727976,-17.1365797057023,75.7199727733194));
#3760=CARTESIAN_POINT('Ctrl Pts',(56.5889518727976,-17.1009015634799,75.7247045904694));
#3761=CARTESIAN_POINT('Ctrl Pts',(56.5889518727976,-16.9340709566345,75.7468232697129));
#3762=CARTESIAN_POINT('Ctrl Pts',(56.5889518727976,-16.6668904840349,75.7802522429883));
#3763=CARTESIAN_POINT('Ctrl Pts',(56.5889518727976,-16.1419971956025,75.8403007103795));
#3764=CARTESIAN_POINT('Ctrl Pts',(56.5889518727976,-15.5057814191354,75.9117619012503));
#3765=CARTESIAN_POINT('Ctrl Pts',(56.5889518727976,-14.9189734632704,76.0160524660517));
#3766=CARTESIAN_POINT('Ctrl Pts',(56.5889518727976,-14.4837747810549,76.144079065061));
#3767=CARTESIAN_POINT('Ctrl Pts',(56.5889518727976,-13.8685280261394,76.387320697005));
#3768=CARTESIAN_POINT('Ctrl Pts',(56.5889518727976,-13.0417655345062,77.0058186775411));
#3769=CARTESIAN_POINT('Ctrl Pts',(56.5889518727977,-12.395995257802,78.1592442349785));
#3770=CARTESIAN_POINT('Ctrl Pts',(56.5889518727976,-12.0948490433455,79.0492977741235));
#3771=CARTESIAN_POINT('Ctrl Pts',(56.5889518727976,-11.9258125052654,79.6651564130096));
#3772=CARTESIAN_POINT('Ctrl Pts',(56.5889518727976,-11.7750493707723,80.4615168367482));
#3773=CARTESIAN_POINT('Ctrl Pts',(56.5889518727976,-11.6854127040116,81.2576240203752));
#3774=CARTESIAN_POINT('Ctrl Pts',(56.5889518727976,-11.629488079385,81.8807180550451));
#3775=CARTESIAN_POINT('Ctrl Pts',(56.5889518727976,-11.5462023151942,82.7966611759654));
#3776=CARTESIAN_POINT('Ctrl Pts',(56.5889518727976,-11.4164595576202,83.802499438733));
#3777=CARTESIAN_POINT('Ctrl Pts',(56.5889518727976,-10.9138529466339,84.8226915242591));
#3778=CARTESIAN_POINT('Ctrl Pts',(56.5889518727976,-10.4060157803267,85.3516937903176));
#3779=CARTESIAN_POINT('Ctrl Pts',(56.5889518727976,-9.89592410072379,85.6871110018963));
#3780=CARTESIAN_POINT('Ctrl Pts',(56.5889518727976,-9.32033135595104,85.9670605844408));
#3781=CARTESIAN_POINT('Ctrl Pts',(56.5889518727976,-8.14723647018877,86.3176571112496));
#3782=CARTESIAN_POINT('Ctrl Pts',(56.5889518727976,-6.84963865195032,86.4137926993747));
#3783=CARTESIAN_POINT('Ctrl Pts',(56.5889518727976,-5.8455592705756,86.3982223088065));
#3784=CARTESIAN_POINT('Ctrl Pts',(57.3635556629615,-17.2540588078706,76.331933813487));
#3785=CARTESIAN_POINT('Ctrl Pts',(57.3635556629615,-17.2183713196357,76.3366670136196));
#3786=CARTESIAN_POINT('Ctrl Pts',(57.3635556629615,-17.1827047092038,76.3413973091119));
#3787=CARTESIAN_POINT('Ctrl Pts',(57.3635556629615,-17.0157846850654,76.3635279934273));
#3788=CARTESIAN_POINT('Ctrl Pts',(57.3635556629616,-16.7417258451673,76.3978253536053));
#3789=CARTESIAN_POINT('Ctrl Pts',(57.3635556629615,-16.2120301045359,76.4583837923497));
#3790=CARTESIAN_POINT('Ctrl Pts',(57.3635556629615,-15.5876752775676,76.5286358687495));
#3791=CARTESIAN_POINT('Ctrl Pts',(57.3635556629616,-15.0552173829869,76.6247643784278));
#3792=CARTESIAN_POINT('Ctrl Pts',(57.3635556629615,-14.6857806853406,76.7334829512476));
#3793=CARTESIAN_POINT('Ctrl Pts',(57.3635556629616,-14.1899011326692,76.931817019722));
#3794=CARTESIAN_POINT('Ctrl Pts',(57.3635556629615,-13.5457125155092,77.4025301809331));
#3795=CARTESIAN_POINT('Ctrl Pts',(57.3635556629616,-12.9646906428169,78.4155180014605));
#3796=CARTESIAN_POINT('Ctrl Pts',(57.3635556629616,-12.6895760107024,79.2313769544293));
#3797=CARTESIAN_POINT('Ctrl Pts',(57.3635556629616,-12.5326496524696,79.8019892501139));
#3798=CARTESIAN_POINT('Ctrl Pts',(57.3635556629616,-12.3906970946281,80.5515523581134));
#3799=CARTESIAN_POINT('Ctrl Pts',(57.3635556629615,-12.3038181611488,81.3191149207297));
#3800=CARTESIAN_POINT('Ctrl Pts',(57.3635556629615,-12.2487289580723,81.9360328998565));
#3801=CARTESIAN_POINT('Ctrl Pts',(57.3635556629615,-12.1636028076754,82.8611187650277));
#3802=CARTESIAN_POINT('Ctrl Pts',(57.3635556629616,-12.033109514969,83.9498819481789));
#3803=CARTESIAN_POINT('Ctrl Pts',(57.3635556629615,-11.4329041685087,85.1834574545092));
#3804=CARTESIAN_POINT('Ctrl Pts',(57.3635556629616,-10.8076443977132,85.8326676190244));
#3805=CARTESIAN_POINT('Ctrl Pts',(57.3635556629616,-10.2014480222085,86.2303334764776));
#3806=CARTESIAN_POINT('Ctrl Pts',(57.3635556629616,-9.53539438980938,86.5536984632034));
#3807=CARTESIAN_POINT('Ctrl Pts',(57.3635556629615,-8.23312149114545,86.9392124383196));
#3808=CARTESIAN_POINT('Ctrl Pts',(57.3635556629615,-6.87250364926861,87.0363166333609));
#3809=CARTESIAN_POINT('Ctrl Pts',(57.3635556629615,-5.83591352823298,87.0202420944917));
#3810=CARTESIAN_POINT('Ctrl Pts',(58.3323903227877,-17.2245457788052,76.109410816774));
#3811=CARTESIAN_POINT('Ctrl Pts',(58.3323903227877,-17.1888582905703,76.1141440169066));
#3812=CARTESIAN_POINT('Ctrl Pts',(58.3323903227877,-17.1531877443463,76.1188747256693));
#3813=CARTESIAN_POINT('Ctrl Pts',(58.3323903227877,-16.9862891793002,76.1410084024959));
#3814=CARTESIAN_POINT('Ctrl Pts',(58.3323903227877,-16.714668593541,76.1750097398116));
#3815=CARTESIAN_POINT('Ctrl Pts',(58.3323903227877,-16.1866358039734,76.2354234730982));
#3816=CARTESIAN_POINT('Ctrl Pts',(58.3323903227877,-15.5579413523181,76.3061735193807));
#3817=CARTESIAN_POINT('Ctrl Pts',(58.3323903227877,-15.0059215204494,76.4053120537038));
#3818=CARTESIAN_POINT('Ctrl Pts',(58.3323903227877,-14.6129386564044,76.5209534522761));
#3819=CARTESIAN_POINT('Ctrl Pts',(58.3323903227877,-14.0742299245444,76.735468440667));
#3820=CARTESIAN_POINT('Ctrl Pts',(58.3323903227877,-13.3646276102391,77.2591022877258));
#3821=CARTESIAN_POINT('Ctrl Pts',(58.3323903227878,-12.7599371622137,78.3228710773516));
#3822=CARTESIAN_POINT('Ctrl Pts',(58.3323903227877,-12.4755009159366,79.165274904841));
#3823=CARTESIAN_POINT('Ctrl Pts',(58.3323903227877,-12.3142252216136,79.7520907812665));
#3824=CARTESIAN_POINT('Ctrl Pts',(58.3323903227877,-12.1691024854386,80.5184246380073));
#3825=CARTESIAN_POINT('Ctrl Pts',(58.3323903227877,-12.0812324563949,81.29621325344));
#3826=CARTESIAN_POINT('Ctrl Pts',(58.3323903227877,-12.0258619451679,81.9153252669056));
#3827=CARTESIAN_POINT('Ctrl Pts',(58.3323903227877,-11.9413735798053,82.8371633715007));
#3828=CARTESIAN_POINT('Ctrl Pts',(58.3323903227877,-11.8116178432401,83.8957997139702));
#3829=CARTESIAN_POINT('Ctrl Pts',(58.3323903227877,-11.2463154451697,85.0530615867849));
#3830=CARTESIAN_POINT('Ctrl Pts',(58.3323903227877,-10.6632413020241,85.6591326134248));
#3831=CARTESIAN_POINT('Ctrl Pts',(58.3323903227877,-10.0914671012367,86.0344931414346));
#3832=CARTESIAN_POINT('Ctrl Pts',(58.3323903227877,-9.45784054547688,86.3422852914887));
#3833=CARTESIAN_POINT('Ctrl Pts',(58.3323903227877,-8.20186765977983,86.7152410304432));
#3834=CARTESIAN_POINT('Ctrl Pts',(58.3323903227877,-6.86436020873407,86.8116917557747));
#3835=CARTESIAN_POINT('Ctrl Pts',(58.3323903227877,-5.83939402043047,86.7957974707539));
#3836=CARTESIAN_POINT('Ctrl Pts',(58.6189035487885,-17.1464005249281,75.5202094835902));
#3837=CARTESIAN_POINT('Ctrl Pts',(58.6189035487885,-17.1107130366932,75.5249426837228));
#3838=CARTESIAN_POINT('Ctrl Pts',(58.6189035487885,-17.0750310537087,75.5296750989469));
#3839=CARTESIAN_POINT('Ctrl Pts',(58.6189035487885,-16.9082380232507,75.5517836790378));
#3840=CARTESIAN_POINT('Ctrl Pts',(58.6189035487886,-16.6432704272489,75.5849231213956));
#3841=CARTESIAN_POINT('Ctrl Pts',(58.6189035487885,-16.119956090455,75.6447764851635));
#3842=CARTESIAN_POINT('Ctrl Pts',(58.6189035487885,-15.480040748791,75.7165669819153));
#3843=CARTESIAN_POINT('Ctrl Pts',(58.6189035487886,-14.8760021144475,75.8233829626469));
#3844=CARTESIAN_POINT('Ctrl Pts',(58.6189035487885,-14.419848797543,75.9575537130432));
#3845=CARTESIAN_POINT('Ctrl Pts',(58.6189035487886,-13.7666435433224,76.2150173339846));
#3846=CARTESIAN_POINT('Ctrl Pts',(58.6189035487885,-12.8817419532219,76.8806007213331));
#3847=CARTESIAN_POINT('Ctrl Pts',(58.6189035487886,-12.2157576301709,78.0783481546451));
#3848=CARTESIAN_POINT('Ctrl Pts',(58.6189035487886,-11.9063174547593,78.9920610457681));
#3849=CARTESIAN_POINT('Ctrl Pts',(58.6189035487886,-11.7334335043027,79.6223345025279));
#3850=CARTESIAN_POINT('Ctrl Pts',(58.6189035487886,-11.5798763077878,80.4335937631608));
#3851=CARTESIAN_POINT('Ctrl Pts',(58.6189035487885,-11.4893640783344,81.238791677157));
#3852=CARTESIAN_POINT('Ctrl Pts',(58.6189035487885,-11.4331579217258,81.8638685679878));
#3853=CARTESIAN_POINT('Ctrl Pts',(58.6189035487885,-11.3504767994824,82.776876201684));
#3854=CARTESIAN_POINT('Ctrl Pts',(58.6189035487885,-11.2205697730928,83.7566656829568));
#3855=CARTESIAN_POINT('Ctrl Pts',(58.6189035487885,-10.7490988661751,84.7087882826478));
#3856=CARTESIAN_POINT('Ctrl Pts',(58.6189035487886,-10.2785552052383,85.1995718651691));
#3857=CARTESIAN_POINT('Ctrl Pts',(58.6189035487886,-9.79907655130654,85.515168675407));
#3858=CARTESIAN_POINT('Ctrl Pts',(58.6189035487886,-9.25227637569268,85.7813082197614));
#3859=CARTESIAN_POINT('Ctrl Pts',(58.6189035487885,-8.12030223033118,86.1208267107997));
#3860=CARTESIAN_POINT('Ctrl Pts',(58.6189035487885,-6.84231551976094,86.2169175365435));
#3861=CARTESIAN_POINT('Ctrl Pts',(58.6189035487885,-5.84860974497664,86.2015080108523));
#3862=CARTESIAN_POINT('Ctrl Pts',(58.6189035487885,-17.1070624647046,75.2236074971792));
#3863=CARTESIAN_POINT('Ctrl Pts',(58.6189035487885,-17.0713749764698,75.2283406973118));
#3864=CARTESIAN_POINT('Ctrl Pts',(58.6189035487885,-17.0356873793413,75.2330738853036));
#3865=CARTESIAN_POINT('Ctrl Pts',(58.6189035487885,-16.868940610655,75.2551744844083));
#3866=CARTESIAN_POINT('Ctrl Pts',(58.6189035487886,-16.6072943602623,75.2878910531892));
#3867=CARTESIAN_POINT('Ctrl Pts',(58.6189035487885,-16.0863108570333,75.3474872987329));
#3868=CARTESIAN_POINT('Ctrl Pts',(58.6189035487885,-15.4407089605501,75.4198407374667));
#3869=CARTESIAN_POINT('Ctrl Pts',(58.6189035487886,-14.810515552782,75.530562741844));
#3870=CARTESIAN_POINT('Ctrl Pts',(58.6189035487885,-14.3226785985763,75.6740330751718));
#3871=CARTESIAN_POINT('Ctrl Pts',(58.6189035487886,-13.6119901077366,75.9531021796814));
#3872=CARTESIAN_POINT('Ctrl Pts',(58.6189035487885,-12.6391386971879,76.6898853504872));
#3873=CARTESIAN_POINT('Ctrl Pts',(58.6189035487886,-11.9421053181931,77.9551448661809));
#3874=CARTESIAN_POINT('Ctrl Pts',(58.6189035487886,-11.620123611833,78.904610366011));
#3875=CARTESIAN_POINT('Ctrl Pts',(58.6189035487886,-11.4414090651326,79.5566822517067));
#3876=CARTESIAN_POINT('Ctrl Pts',(58.6189035487886,-11.283611680672,80.3904836204666));
#3877=CARTESIAN_POINT('Ctrl Pts',(58.6189035487885,-11.191771906312,81.2094324300899));
#3878=CARTESIAN_POINT('Ctrl Pts',(58.6189035487885,-11.1351578812696,81.8374901150816));
#3879=CARTESIAN_POINT('Ctrl Pts',(58.6189035487885,-11.053369822089,82.7460850644104));
#3880=CARTESIAN_POINT('Ctrl Pts',(58.6189035487885,-10.9236831233095,83.6860531538696));
#3881=CARTESIAN_POINT('Ctrl Pts',(58.6189035487885,-10.4992473440377,84.5353425071605));
#3882=CARTESIAN_POINT('Ctrl Pts',(58.6189035487886,-10.0852341421502,84.9682405076987));
#3883=CARTESIAN_POINT('Ctrl Pts',(58.6189035487886,-9.65205447547462,85.2538515396933));
#3884=CARTESIAN_POINT('Ctrl Pts',(58.6189035487886,-9.1488264052405,85.4990822689984));
#3885=CARTESIAN_POINT('Ctrl Pts',(58.6189035487885,-8.07907491053992,85.8217946659718));
#3886=CARTESIAN_POINT('Ctrl Pts',(58.6189035487885,-6.83128625461351,85.9175112317093));
#3887=CARTESIAN_POINT('Ctrl Pts',(58.6189035487885,-5.85324890998301,85.9023446784181));
#3888=CARTESIAN_POINT('Ctrl Pts',(56.7143685644419,-17.0504395293355,74.7966806225093));
#3889=CARTESIAN_POINT('Ctrl Pts',(56.7149839995477,-17.0502694819401,74.795398495354));
#3890=CARTESIAN_POINT('Ctrl Pts',(56.7156024450586,-17.0500996228054,74.7941177876506));
#3891=CARTESIAN_POINT('Ctrl Pts',(56.7162239011616,-17.0499299537481,74.7928385130966));
#3892=CARTESIAN_POINT('Ctrl Pts',(56.8455023604483,-17.0146345334931,74.5267173139489));
#3893=CARTESIAN_POINT('Ctrl Pts',(57.1050624944829,-16.9875646029503,74.3226148461249));
#3894=CARTESIAN_POINT('Ctrl Pts',(57.396117357852,-16.9788276685414,74.2567399126353));
#3895=CARTESIAN_POINT('Ctrl Pts',(57.6696862862663,-16.970615629903,74.1948226000178));
#3896=CARTESIAN_POINT('Ctrl Pts',(57.9710793513523,-16.9785999454106,74.2550229206802));
#3897=CARTESIAN_POINT('Ctrl Pts',(58.1997282611953,-16.9998571535647,74.4152984942149));
#3898=CARTESIAN_POINT('Origin',(57.6189035487885,-17.,75.237807097577));
#3899=CARTESIAN_POINT('',(58.6189035487885,-5.85324890998301,85.9023446784181));
#3900=CARTESIAN_POINT('Ctrl Pts',(58.6189035487885,-17.0000000161406,75.2378038846518));
#3901=CARTESIAN_POINT('Ctrl Pts',(58.6189035487885,-16.868940610655,75.2551744844083));
#3902=CARTESIAN_POINT('Ctrl Pts',(58.6189035487886,-16.6072943602623,75.2878910531892));
#3903=CARTESIAN_POINT('Ctrl Pts',(58.6189035487885,-16.0863108570333,75.3474872987329));
#3904=CARTESIAN_POINT('Ctrl Pts',(58.6189035487885,-15.4407089605501,75.4198407374667));
#3905=CARTESIAN_POINT('Ctrl Pts',(58.6189035487886,-14.810515552782,75.530562741844));
#3906=CARTESIAN_POINT('Ctrl Pts',(58.6189035487885,-14.3226785985763,75.6740330751718));
#3907=CARTESIAN_POINT('Ctrl Pts',(58.6189035487886,-13.6119901077366,75.9531021796814));
#3908=CARTESIAN_POINT('Ctrl Pts',(58.6189035487885,-12.6391386971879,76.6898853504872));
#3909=CARTESIAN_POINT('Ctrl Pts',(58.6189035487886,-11.9421053181931,77.9551448661809));
#3910=CARTESIAN_POINT('Ctrl Pts',(58.6189035487886,-11.620123611833,78.904610366011));
#3911=CARTESIAN_POINT('Ctrl Pts',(58.6189035487886,-11.4414090651326,79.5566822517067));
#3912=CARTESIAN_POINT('Ctrl Pts',(58.6189035487886,-11.283611680672,80.3904836204666));
#3913=CARTESIAN_POINT('Ctrl Pts',(58.6189035487885,-11.191771906312,81.2094324300899));
#3914=CARTESIAN_POINT('Ctrl Pts',(58.6189035487885,-11.1351578812696,81.8374901150816));
#3915=CARTESIAN_POINT('Ctrl Pts',(58.6189035487885,-11.053369822089,82.7460850644104));
#3916=CARTESIAN_POINT('Ctrl Pts',(58.6189035487885,-10.9236831233095,83.6860531538696));
#3917=CARTESIAN_POINT('Ctrl Pts',(58.6189035487885,-10.4992473440377,84.5353425071605));
#3918=CARTESIAN_POINT('Ctrl Pts',(58.6189035487886,-10.0852341421502,84.9682405076987));
#3919=CARTESIAN_POINT('Ctrl Pts',(58.6189035487886,-9.65205447547462,85.2538515396933));
#3920=CARTESIAN_POINT('Ctrl Pts',(58.6189035487886,-9.1488264052405,85.4990822689984));
#3921=CARTESIAN_POINT('Ctrl Pts',(58.6189035487885,-8.07907491053992,85.8217946659718));
#3922=CARTESIAN_POINT('Ctrl Pts',(58.6189035487885,-6.83128625461351,85.9175112317093));
#3923=CARTESIAN_POINT('Ctrl Pts',(58.6189035487885,-5.85324890998301,85.9023446784181));
#3924=CARTESIAN_POINT('Origin',(57.6189035487885,-5.85324890998301,85.9023446784181));
#3925=CARTESIAN_POINT('Ctrl Pts',(57.0348213440502,-17.1658500115857,49.3940081933445));
#3926=CARTESIAN_POINT('Ctrl Pts',(57.036896662294,-17.1105926457513,49.4039659001254));
#3927=CARTESIAN_POINT('Ctrl Pts',(57.0379346870417,-17.0552963237907,49.4139236069063));
#3928=CARTESIAN_POINT('Ctrl Pts',(57.0379346870417,-17.,49.4238813136872));
#3929=CARTESIAN_POINT('Ctrl Pts',(56.8725534287442,-17.1597556645255,49.509914425448));
#3930=CARTESIAN_POINT('Ctrl Pts',(56.874552252259,-17.1065350452187,49.5198721322289));
#3931=CARTESIAN_POINT('Ctrl Pts',(56.8755523684112,-17.0532581413011,49.5298298390098));
#3932=CARTESIAN_POINT('Ctrl Pts',(56.8755523684112,-17.,49.5397875457908));
#3933=CARTESIAN_POINT('Ctrl Pts',(56.6199907504015,-17.1502700886903,49.8416628129442));
#3934=CARTESIAN_POINT('Ctrl Pts',(56.6218712933677,-17.100198803981,49.8516205197251));
#3935=CARTESIAN_POINT('Ctrl Pts',(56.6228116264629,-17.0501065863364,49.861578226506));
#3936=CARTESIAN_POINT('Ctrl Pts',(56.6228116264629,-17.,49.8715359332869));
#3937=CARTESIAN_POINT('Ctrl Pts',(56.5976270641714,-17.1494301687025,50.2581169344504));
#3938=CARTESIAN_POINT('Ctrl Pts',(56.5994965856415,-17.0996523420419,50.2680746412313));
#3939=CARTESIAN_POINT('Ctrl Pts',(56.6004321732215,-17.0498129213918,50.2780323480122));
#3940=CARTESIAN_POINT('Ctrl Pts',(56.6004321732215,-17.,50.2879900547931));
#3941=CARTESIAN_POINT('Ctrl Pts',(56.6462070845395,-17.1512547037855,50.4516083418488));
#3942=CARTESIAN_POINT('Ctrl Pts',(56.6480997684365,-17.1008601549921,50.4615660486297));
#3943=CARTESIAN_POINT('Ctrl Pts',(56.6490464438345,-17.0504300783306,50.4715237554107));
#3944=CARTESIAN_POINT('Ctrl Pts',(56.6490464438345,-17.,50.4814814621916));
#3945=CARTESIAN_POINT('Origin',(57.6189035487885,-17.,50.237807097577));
#3946=CARTESIAN_POINT('Origin',(57.6189035487885,-17.,50.237807097577));
#3947=CARTESIAN_POINT('Origin',(57.6189035487885,-21.7910956063159,41.2894961290256));
#3948=CARTESIAN_POINT('Origin',(57.6189035487885,-17.1070624647042,75.2236074971793));
#3949=CARTESIAN_POINT('',(57.6189035487885,-17.,74.4163755309633));
#3950=CARTESIAN_POINT('Origin',(57.6189035487885,-17.,75.237807097577));
#3951=CARTESIAN_POINT('Origin',(57.6189035487885,-5.85324890998301,85.9023446784181));
#3952=CARTESIAN_POINT('Origin',(57.6189035487885,-17.,75.237807097577));
#3953=CARTESIAN_POINT('',(0.,0.,0.));
#3954=CARTESIAN_POINT('Origin',(-0.00360820116592981,5.,47.167824608198));
#3955=CARTESIAN_POINT('',(-14.4855638369713,0.,47.167824608198));
#3956=CARTESIAN_POINT('Origin',(-0.00360820116592981,0.,47.167824608198));
#3957=CARTESIAN_POINT('',(-14.4855638369713,5.,47.167824608198));
#3958=CARTESIAN_POINT('',(-14.4855638369713,5.,47.167824608198));
#3959=CARTESIAN_POINT('Origin',(-0.00360820116592981,5.,47.167824608198));
#3960=CARTESIAN_POINT('Origin',(-0.00360820116592981,5.,47.167824608198));
#3961=CARTESIAN_POINT('',(-17.4855638369713,0.,47.167824608198));
#3962=CARTESIAN_POINT('Origin',(-0.00360820116592981,0.,47.167824608198));
#3963=CARTESIAN_POINT('',(-17.4855638369713,5.,47.167824608198));
#3964=CARTESIAN_POINT('',(-17.4855638369713,5.,47.167824608198));
#3965=CARTESIAN_POINT('Origin',(-0.00360820116592981,5.,47.167824608198));
#3966=CARTESIAN_POINT('Origin',(-0.00360820116592997,0.,47.167824608198));
#3967=CARTESIAN_POINT('Origin',(-0.00360820116592997,5.,47.167824608198));
#3968=CARTESIAN_POINT('',(0.,0.,0.));
#3969=CARTESIAN_POINT('Origin',(73.2288574389116,5.,87.4952777324745));
#3970=CARTESIAN_POINT('',(67.2288574389116,-10.,87.4952777324745));
#3971=CARTESIAN_POINT('Origin',(73.2288574389116,-10.,87.4952777324745));
#3972=CARTESIAN_POINT('',(67.2288574389116,5.,87.4952777324745));
#3973=CARTESIAN_POINT('',(67.2288574389116,5.,87.4952777324745));
#3974=CARTESIAN_POINT('Origin',(73.2288574389116,5.,87.4952777324745));
#3975=CARTESIAN_POINT('Origin',(73.2288574389116,-10.,87.4952777324745));
#3976=CARTESIAN_POINT('Origin',(73.2288574389116,5.,87.4952777324745));
#3977=CARTESIAN_POINT('',(0.,0.,0.));
#3978=CARTESIAN_POINT('Origin',(59.5698926278372,-18.,39.6167831756372));
#3979=CARTESIAN_POINT('',(66.5698926278372,-18.,44.4641879853147));
#3980=CARTESIAN_POINT('',(59.5698926278372,-25.,44.4641879853147));
#3981=CARTESIAN_POINT('Origin',(59.5698926278372,-18.,44.4641879853147));
#3982=CARTESIAN_POINT('',(59.5698926278372,-25.,38.0009815724114));
#3983=CARTESIAN_POINT('',(59.5698926278372,-25.,39.6167831756372));
#3984=CARTESIAN_POINT('',(66.5698926278372,-18.,38.0009815724114));
#3985=CARTESIAN_POINT('Origin',(59.5698926278372,-18.,38.0009815724114));
#3986=CARTESIAN_POINT('',(66.5698926278372,-18.,39.6167831756372));
#3987=CARTESIAN_POINT('Origin',(57.9894289417414,-25.,41.2325847788631));
#3988=CARTESIAN_POINT('',(56.4089652556457,-25.,44.4641879853147));
#3989=CARTESIAN_POINT('',(49.4089652556457,-25.,44.4641879853147));
#3990=CARTESIAN_POINT('',(56.4089652556457,-25.,38.0009815724114));
#3991=CARTESIAN_POINT('',(56.4089652556457,-25.,42.8483863820889));
#3992=CARTESIAN_POINT('',(66.5698926278372,-25.,38.0009815724114));
#3993=CARTESIAN_POINT('Origin',(66.5698926278372,5.,44.4641879853147));
#3994=CARTESIAN_POINT('',(66.5698926278372,5.,44.4641879853147));
#3995=CARTESIAN_POINT('',(66.5698926278372,5.,44.4641879853147));
#3996=CARTESIAN_POINT('',(49.4089652556457,5.,44.4641879853147));
#3997=CARTESIAN_POINT('',(49.4089652556457,5.,44.4641879853147));
#3998=CARTESIAN_POINT('',(49.4089652556457,-18.,44.4641879853147));
#3999=CARTESIAN_POINT('',(49.4089652556457,5.,44.4641879853147));
#4000=CARTESIAN_POINT('Origin',(56.4089652556457,-18.,44.4641879853147));
#4001=CARTESIAN_POINT('Origin',(56.4089652556457,-18.,42.8483863820889));
#4002=CARTESIAN_POINT('',(49.4089652556457,-18.,38.0009815724114));
#4003=CARTESIAN_POINT('Origin',(56.4089652556457,-18.,38.0009815724114));
#4004=CARTESIAN_POINT('',(49.4089652556457,-18.,42.8483863820889));
#4005=CARTESIAN_POINT('Origin',(49.4089652556457,5.,38.0009815724114));
#4006=CARTESIAN_POINT('',(49.4089652556457,5.,38.0009815724114));
#4007=CARTESIAN_POINT('',(49.4089652556457,5.,38.0009815724114));
#4008=CARTESIAN_POINT('',(66.5698926278372,5.,38.0009815724114));
#4009=CARTESIAN_POINT('',(66.5698926278372,5.,38.0009815724114));
#4010=CARTESIAN_POINT('',(66.5698926278372,5.,38.0009815724114));
#4011=CARTESIAN_POINT('Origin',(49.4089652556457,5.,44.4641879853147));
#4012=CARTESIAN_POINT('',(49.4089652556457,5.,38.0009815724114));
#4013=CARTESIAN_POINT('Origin',(66.5698926278372,5.,38.0009815724114));
#4014=CARTESIAN_POINT('',(66.5698926278372,5.,44.4641879853147));
#4015=CARTESIAN_POINT('Origin',(57.9894289417414,5.,41.2325847788631));
#4016=CARTESIAN_POINT('',(0.,0.,0.));
#4017=CARTESIAN_POINT('Origin',(101.305059905209,5.,116.266583003001));
#4018=CARTESIAN_POINT('',(101.305059905209,5.,0.));
#4019=CARTESIAN_POINT('',(101.305059905209,5.,116.266583003001));
#4020=CARTESIAN_POINT('',(101.305059905209,5.,0.));
#4021=CARTESIAN_POINT('',(101.305059905209,15.,0.));
#4022=CARTESIAN_POINT('',(101.305059905209,5.,0.));
#4023=CARTESIAN_POINT('',(101.305059905209,15.,116.266583003001));
#4024=CARTESIAN_POINT('',(101.305059905209,15.,0.));
#4025=CARTESIAN_POINT('',(101.305059905209,5.,116.266583003001));
#4026=CARTESIAN_POINT('Origin',(-67.8619652977995,5.,116.266583003001));
#4027=CARTESIAN_POINT('',(-67.8619652977995,5.,116.266583003001));
#4028=CARTESIAN_POINT('',(101.305059905209,5.,116.266583003001));
#4029=CARTESIAN_POINT('',(-67.8619652977995,15.,116.266583003001));
#4030=CARTESIAN_POINT('',(101.305059905209,15.,116.266583003001));
#4031=CARTESIAN_POINT('',(-67.8619652977995,5.,116.266583003001));
#4032=CARTESIAN_POINT('Origin',(-67.8619652977995,5.,0.));
#4033=CARTESIAN_POINT('',(-67.8619652977995,5.,0.));
#4034=CARTESIAN_POINT('',(-67.8619652977995,5.,116.266583003001));
#4035=CARTESIAN_POINT('',(-67.8619652977995,15.,0.));
#4036=CARTESIAN_POINT('',(-67.8619652977995,15.,116.266583003001));
#4037=CARTESIAN_POINT('',(-67.8619652977995,5.,0.));
#4038=CARTESIAN_POINT('Origin',(101.305059905209,5.,0.));
#4039=CARTESIAN_POINT('',(-67.8619652977995,5.,0.));
#4040=CARTESIAN_POINT('',(-67.8619652977995,15.,0.));
#4041=CARTESIAN_POINT('Origin',(16.721547303705,15.,58.1332915015007));
#4042=CARTESIAN_POINT('Origin',(16.721547303705,5.,58.1332915015007));
#4043=CARTESIAN_POINT('',(0.,0.,0.));
#4044=CARTESIAN_POINT('Origin',(-0.00360820116592981,5.,47.167824608198));
#4045=CARTESIAN_POINT('',(-14.4855638369713,-10.,47.167824608198));
#4046=CARTESIAN_POINT('Origin',(-0.00360820116592981,-10.,47.167824608198));
#4047=CARTESIAN_POINT('',(-14.4855638369713,5.,47.167824608198));
#4048=CARTESIAN_POINT('',(-14.4855638369713,5.,47.167824608198));
#4049=CARTESIAN_POINT('Origin',(-0.00360820116592981,5.,47.167824608198));
#4050=CARTESIAN_POINT('Origin',(-0.00360820116592997,-10.,47.167824608198));
#4051=CARTESIAN_POINT('Origin',(-0.00360820116592997,5.,47.167824608198));
#4052=CARTESIAN_POINT('',(0.,0.,0.));
#4053=CARTESIAN_POINT('',(0.,0.,0.));
#4054=CARTESIAN_POINT('',(0.,0.,0.));
#4055=CARTESIAN_POINT('',(0.,0.,0.));
#4056=CARTESIAN_POINT('',(0.,0.,0.));
#4057=CARTESIAN_POINT('',(0.,0.,0.));
#4058=CARTESIAN_POINT('',(0.,0.,0.));
#4059=CARTESIAN_POINT('',(0.,0.,0.));
#4060=UNCERTAINTY_MEASURE_WITH_UNIT(LENGTH_MEASURE(0.01),#4080,
'DISTANCE_ACCURACY_VALUE',
'Maximum model space distance between geometric entities at asserted c
onnectivities');
#4061=UNCERTAINTY_MEASURE_WITH_UNIT(LENGTH_MEASURE(0.01),#4080,
'DISTANCE_ACCURACY_VALUE',
'Maximum model space distance between geometric entities at asserted c
onnectivities');
#4062=UNCERTAINTY_MEASURE_WITH_UNIT(LENGTH_MEASURE(0.01),#4080,
'DISTANCE_ACCURACY_VALUE',
'Maximum model space distance between geometric entities at asserted c
onnectivities');
#4063=UNCERTAINTY_MEASURE_WITH_UNIT(LENGTH_MEASURE(0.01),#4080,
'DISTANCE_ACCURACY_VALUE',
'Maximum model space distance between geometric entities at asserted c
onnectivities');
#4064=UNCERTAINTY_MEASURE_WITH_UNIT(LENGTH_MEASURE(0.01),#4080,
'DISTANCE_ACCURACY_VALUE',
'Maximum model space distance between geometric entities at asserted c
onnectivities');
#4065=UNCERTAINTY_MEASURE_WITH_UNIT(LENGTH_MEASURE(0.01),#4080,
'DISTANCE_ACCURACY_VALUE',
'Maximum model space distance between geometric entities at asserted c
onnectivities');
#4066=UNCERTAINTY_MEASURE_WITH_UNIT(LENGTH_MEASURE(0.01),#4080,
'DISTANCE_ACCURACY_VALUE',
'Maximum model space distance between geometric entities at asserted c
onnectivities');
#4067=UNCERTAINTY_MEASURE_WITH_UNIT(LENGTH_MEASURE(0.01),#4080,
'DISTANCE_ACCURACY_VALUE',
'Maximum model space distance between geometric entities at asserted c
onnectivities');
#4068=UNCERTAINTY_MEASURE_WITH_UNIT(LENGTH_MEASURE(0.01),#4080,
'DISTANCE_ACCURACY_VALUE',
'Maximum model space distance between geometric entities at asserted c
onnectivities');
#4069=UNCERTAINTY_MEASURE_WITH_UNIT(LENGTH_MEASURE(0.01),#4080,
'DISTANCE_ACCURACY_VALUE',
'Maximum model space distance between geometric entities at asserted c
onnectivities');
#4070=(
GEOMETRIC_REPRESENTATION_CONTEXT(3)
GLOBAL_UNCERTAINTY_ASSIGNED_CONTEXT((#4060))
GLOBAL_UNIT_ASSIGNED_CONTEXT((#4080,#4082,#4083))
REPRESENTATION_CONTEXT('','3D')
);
#4071=(
GEOMETRIC_REPRESENTATION_CONTEXT(3)
GLOBAL_UNCERTAINTY_ASSIGNED_CONTEXT((#4061))
GLOBAL_UNIT_ASSIGNED_CONTEXT((#4080,#4082,#4083))
REPRESENTATION_CONTEXT('','3D')
);
#4072=(
GEOMETRIC_REPRESENTATION_CONTEXT(3)
GLOBAL_UNCERTAINTY_ASSIGNED_CONTEXT((#4062))
GLOBAL_UNIT_ASSIGNED_CONTEXT((#4080,#4082,#4083))
REPRESENTATION_CONTEXT('','3D')
);
#4073=(
GEOMETRIC_REPRESENTATION_CONTEXT(3)
GLOBAL_UNCERTAINTY_ASSIGNED_CONTEXT((#4063))
GLOBAL_UNIT_ASSIGNED_CONTEXT((#4080,#4082,#4083))
REPRESENTATION_CONTEXT('','3D')
);
#4074=(
GEOMETRIC_REPRESENTATION_CONTEXT(3)
GLOBAL_UNCERTAINTY_ASSIGNED_CONTEXT((#4064))
GLOBAL_UNIT_ASSIGNED_CONTEXT((#4080,#4082,#4083))
REPRESENTATION_CONTEXT('','3D')
);
#4075=(
GEOMETRIC_REPRESENTATION_CONTEXT(3)
GLOBAL_UNCERTAINTY_ASSIGNED_CONTEXT((#4065))
GLOBAL_UNIT_ASSIGNED_CONTEXT((#4080,#4082,#4083))
REPRESENTATION_CONTEXT('','3D')
);
#4076=(
GEOMETRIC_REPRESENTATION_CONTEXT(3)
GLOBAL_UNCERTAINTY_ASSIGNED_CONTEXT((#4066))
GLOBAL_UNIT_ASSIGNED_CONTEXT((#4080,#4082,#4083))
REPRESENTATION_CONTEXT('','3D')
);
#4077=(
GEOMETRIC_REPRESENTATION_CONTEXT(3)
GLOBAL_UNCERTAINTY_ASSIGNED_CONTEXT((#4067))
GLOBAL_UNIT_ASSIGNED_CONTEXT((#4080,#4082,#4083))
REPRESENTATION_CONTEXT('','3D')
);
#4078=(
GEOMETRIC_REPRESENTATION_CONTEXT(3)
GLOBAL_UNCERTAINTY_ASSIGNED_CONTEXT((#4068))
GLOBAL_UNIT_ASSIGNED_CONTEXT((#4080,#4082,#4083))
REPRESENTATION_CONTEXT('','3D')
);
#4079=(
GEOMETRIC_REPRESENTATION_CONTEXT(3)
GLOBAL_UNCERTAINTY_ASSIGNED_CONTEXT((#4069))
GLOBAL_UNIT_ASSIGNED_CONTEXT((#4080,#4082,#4083))
REPRESENTATION_CONTEXT('','3D')
);
#4080=(
LENGTH_UNIT()
NAMED_UNIT(*)
SI_UNIT(.MILLI.,.METRE.)
);
#4081=(
LENGTH_UNIT()
NAMED_UNIT(*)
SI_UNIT($,.METRE.)
);
#4082=(
NAMED_UNIT(*)
PLANE_ANGLE_UNIT()
SI_UNIT($,.RADIAN.)
);
#4083=(
NAMED_UNIT(*)
SI_UNIT($,.STERADIAN.)
SOLID_ANGLE_UNIT()
);
#4084=SHAPE_DEFINITION_REPRESENTATION(#4093,#4110);
#4085=SHAPE_DEFINITION_REPRESENTATION(#4094,#4111);
#4086=SHAPE_DEFINITION_REPRESENTATION(#4095,#4112);
#4087=SHAPE_DEFINITION_REPRESENTATION(#4096,#4113);
#4088=SHAPE_DEFINITION_REPRESENTATION(#4097,#4114);
#4089=SHAPE_DEFINITION_REPRESENTATION(#4098,#4115);
#4090=SHAPE_DEFINITION_REPRESENTATION(#4099,#4116);
#4091=SHAPE_DEFINITION_REPRESENTATION(#4100,#4117);
#4092=SHAPE_DEFINITION_REPRESENTATION(#4101,#4118);
#4093=PRODUCT_DEFINITION_SHAPE('',$,#4120);
#4094=PRODUCT_DEFINITION_SHAPE('',$,#4121);
#4095=PRODUCT_DEFINITION_SHAPE('',$,#4122);
#4096=PRODUCT_DEFINITION_SHAPE('',$,#4123);
#4097=PRODUCT_DEFINITION_SHAPE('',$,#4124);
#4098=PRODUCT_DEFINITION_SHAPE('',$,#4125);
#4099=PRODUCT_DEFINITION_SHAPE('',$,#4126);
#4100=PRODUCT_DEFINITION_SHAPE('',$,#4127);
#4101=PRODUCT_DEFINITION_SHAPE('',$,#4128);
#4102=PRODUCT_DEFINITION_SHAPE($,$,#35);
#4103=PRODUCT_DEFINITION_SHAPE($,$,#36);
#4104=PRODUCT_DEFINITION_SHAPE($,$,#37);
#4105=PRODUCT_DEFINITION_SHAPE($,$,#38);
#4106=PRODUCT_DEFINITION_SHAPE($,$,#39);
#4107=PRODUCT_DEFINITION_SHAPE($,$,#40);
#4108=PRODUCT_DEFINITION_SHAPE($,$,#41);
#4109=PRODUCT_DEFINITION_SHAPE($,$,#42);
#4110=SHAPE_REPRESENTATION('',(#1540,#1690,#1691,#1692,#1693,#1694,#1695,
#1696,#1697),#4070);
#4111=SHAPE_REPRESENTATION('',(#1541),#4071);
#4112=SHAPE_REPRESENTATION('',(#1619),#4072);
#4113=SHAPE_REPRESENTATION('',(#1632),#4073);
#4114=SHAPE_REPRESENTATION('',(#1649),#4074);
#4115=SHAPE_REPRESENTATION('',(#1658),#4075);
#4116=SHAPE_REPRESENTATION('',(#1664),#4076);
#4117=SHAPE_REPRESENTATION('',(#1677),#4077);
#4118=SHAPE_REPRESENTATION('',(#1684),#4078);
#4119=PRODUCT_DEFINITION_CONTEXT('part definition',#4148,'design');
#4120=PRODUCT_DEFINITION('BR-055','BR-055',#4129,#4119);
#4121=PRODUCT_DEFINITION('Wheel','Wheel',#4130,#4119);
#4122=PRODUCT_DEFINITION('Pawl','Pawl',#4131,#4119);
#4123=PRODUCT_DEFINITION('Spring','Spring',#4132,#4119);
#4124=PRODUCT_DEFINITION('Spacer','Spacer',#4133,#4119);
#4125=PRODUCT_DEFINITION('Pin_02','Pin_02',#4134,#4119);
#4126=PRODUCT_DEFINITION('Spring_Holder','Spring_Holder',#4135,#4119);
#4127=PRODUCT_DEFINITION('Base','Base',#4136,#4119);
#4128=PRODUCT_DEFINITION('Pin_01','Pin_01',#4137,#4119);
#4129=PRODUCT_DEFINITION_FORMATION('',$,#4150);
#4130=PRODUCT_DEFINITION_FORMATION('',$,#4151);
#4131=PRODUCT_DEFINITION_FORMATION('',$,#4152);
#4132=PRODUCT_DEFINITION_FORMATION('',$,#4153);
#4133=PRODUCT_DEFINITION_FORMATION('',$,#4154);
#4134=PRODUCT_DEFINITION_FORMATION('',$,#4155);
#4135=PRODUCT_DEFINITION_FORMATION('',$,#4156);
#4136=PRODUCT_DEFINITION_FORMATION('',$,#4157);
#4137=PRODUCT_DEFINITION_FORMATION('',$,#4158);
#4138=PRODUCT_RELATED_PRODUCT_CATEGORY('BR-055','BR-055',(#4150));
#4139=PRODUCT_RELATED_PRODUCT_CATEGORY('Wheel','Wheel',(#4151));
#4140=PRODUCT_RELATED_PRODUCT_CATEGORY('Pawl','Pawl',(#4152));
#4141=PRODUCT_RELATED_PRODUCT_CATEGORY('Spring','Spring',(#4153));
#4142=PRODUCT_RELATED_PRODUCT_CATEGORY('Spacer','Spacer',(#4154));
#4143=PRODUCT_RELATED_PRODUCT_CATEGORY('Pin_02','Pin_02',(#4155));
#4144=PRODUCT_RELATED_PRODUCT_CATEGORY('Spring_Holder','Spring_Holder',
(#4156));
#4145=PRODUCT_RELATED_PRODUCT_CATEGORY('Base','Base',(#4157));
#4146=PRODUCT_RELATED_PRODUCT_CATEGORY('Pin_01','Pin_01',(#4158));
#4147=APPLICATION_PROTOCOL_DEFINITION('international standard',
'automotive_design',2009,#4148);
#4148=APPLICATION_CONTEXT(
'Core Data for Automotive Mechanical Design Process');
#4149=PRODUCT_CONTEXT('part definition',#4148,'mechanical');
#4150=PRODUCT('BR-055','BR-055',$,(#4149));
#4151=PRODUCT('Wheel','Wheel',$,(#4149));
#4152=PRODUCT('Pawl','Pawl',$,(#4149));
#4153=PRODUCT('Spring','Spring',$,(#4149));
#4154=PRODUCT('Spacer','Spacer',$,(#4149));
#4155=PRODUCT('Pin_02','Pin_02',$,(#4149));
#4156=PRODUCT('Spring_Holder','Spring_Holder',$,(#4149));
#4157=PRODUCT('Base','Base',$,(#4149));
#4158=PRODUCT('Pin_01','Pin_01',$,(#4149));
#4159=PRESENTATION_STYLE_ASSIGNMENT((#4163));
#4160=PRESENTATION_STYLE_ASSIGNMENT((#4164));
#4161=PRESENTATION_STYLE_ASSIGNMENT((#4165));
#4162=PRESENTATION_STYLE_ASSIGNMENT((#4166));
#4163=SURFACE_STYLE_USAGE(.BOTH.,#4167);
#4164=SURFACE_STYLE_USAGE(.BOTH.,#4168);
#4165=SURFACE_STYLE_USAGE(.BOTH.,#4169);
#4166=SURFACE_STYLE_USAGE(.BOTH.,#4170);
#4167=SURFACE_SIDE_STYLE('',(#4171));
#4168=SURFACE_SIDE_STYLE('',(#4172));
#4169=SURFACE_SIDE_STYLE('',(#4173));
#4170=SURFACE_SIDE_STYLE('',(#4174));
#4171=SURFACE_STYLE_FILL_AREA(#4175);
#4172=SURFACE_STYLE_FILL_AREA(#4176);
#4173=SURFACE_STYLE_FILL_AREA(#4177);
#4174=SURFACE_STYLE_FILL_AREA(#4178);
#4175=FILL_AREA_STYLE('Steel - Satin',(#4179));
#4176=FILL_AREA_STYLE('Stainless Steel - Polished',(#4180));
#4177=FILL_AREA_STYLE('Stainless Steel - Polished',(#4181));
#4178=FILL_AREA_STYLE('Stainless Steel - Satin',(#4182));
#4179=FILL_AREA_STYLE_COLOUR('Steel - Satin',#4183);
#4180=FILL_AREA_STYLE_COLOUR('Stainless Steel - Polished',#4184);
#4181=FILL_AREA_STYLE_COLOUR('Stainless Steel - Polished',#4185);
#4182=FILL_AREA_STYLE_COLOUR('Stainless Steel - Satin',#4186);
#4183=COLOUR_RGB('Steel - Satin', 0.40784314, 0.44705882, 0.49803922);
#4184=COLOUR_RGB('Stainless Steel - Polished', 0.09019608, 0.27058824, 0.51372549);
#4185=COLOUR_RGB('Stainless Steel - Polished', 0.66274510, 0.83137255, 0.94901961);
#4186=COLOUR_RGB('Stainless Steel - Satin', 0.31764706, 0.68627451, 0.89019608);
ENDSEC;
END-ISO-10303-21;
